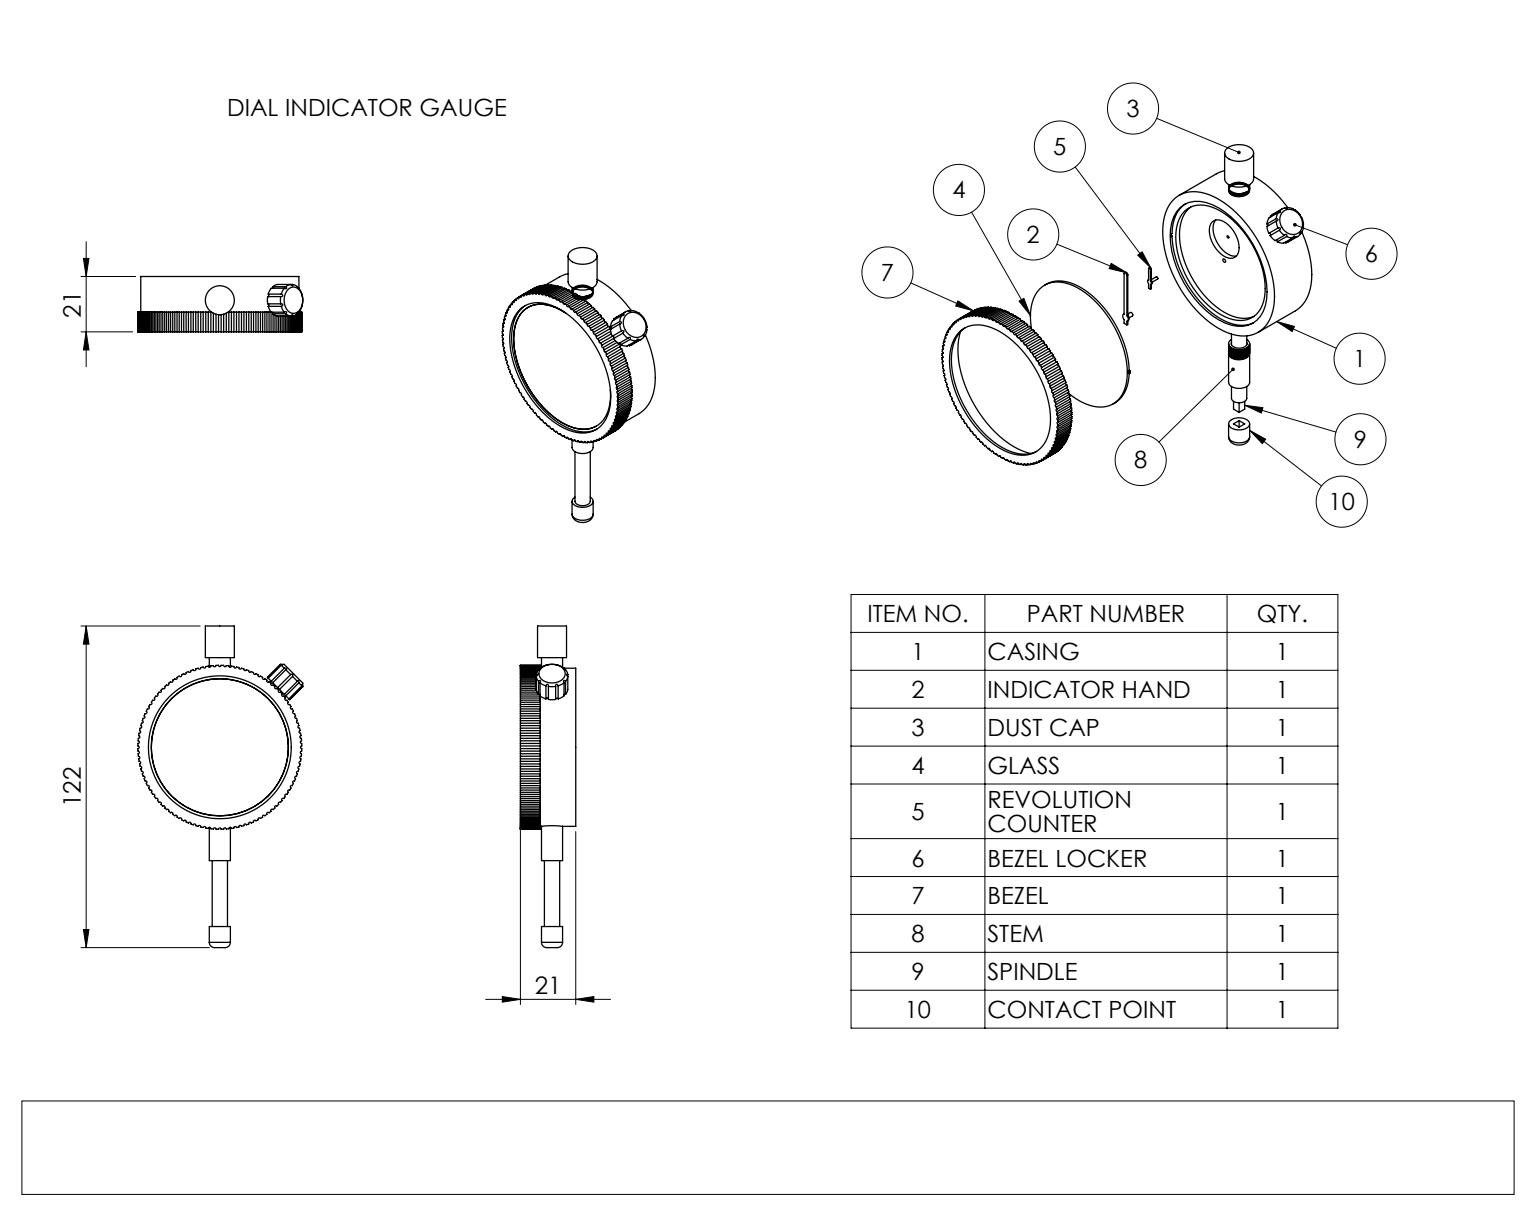
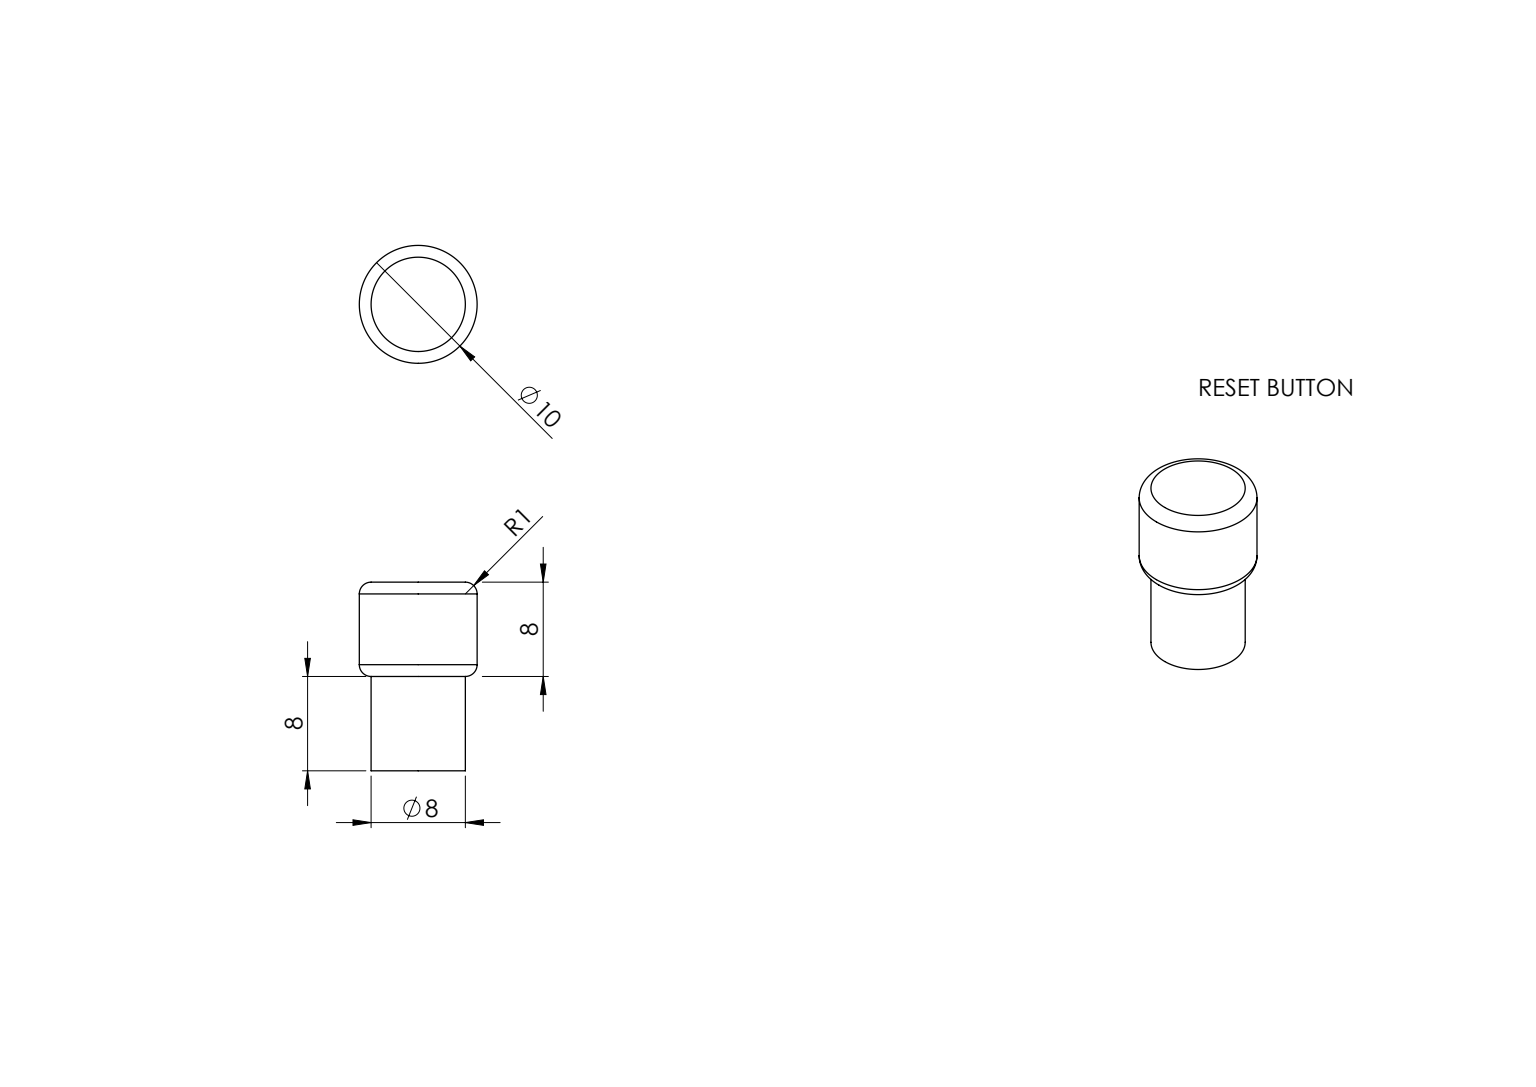
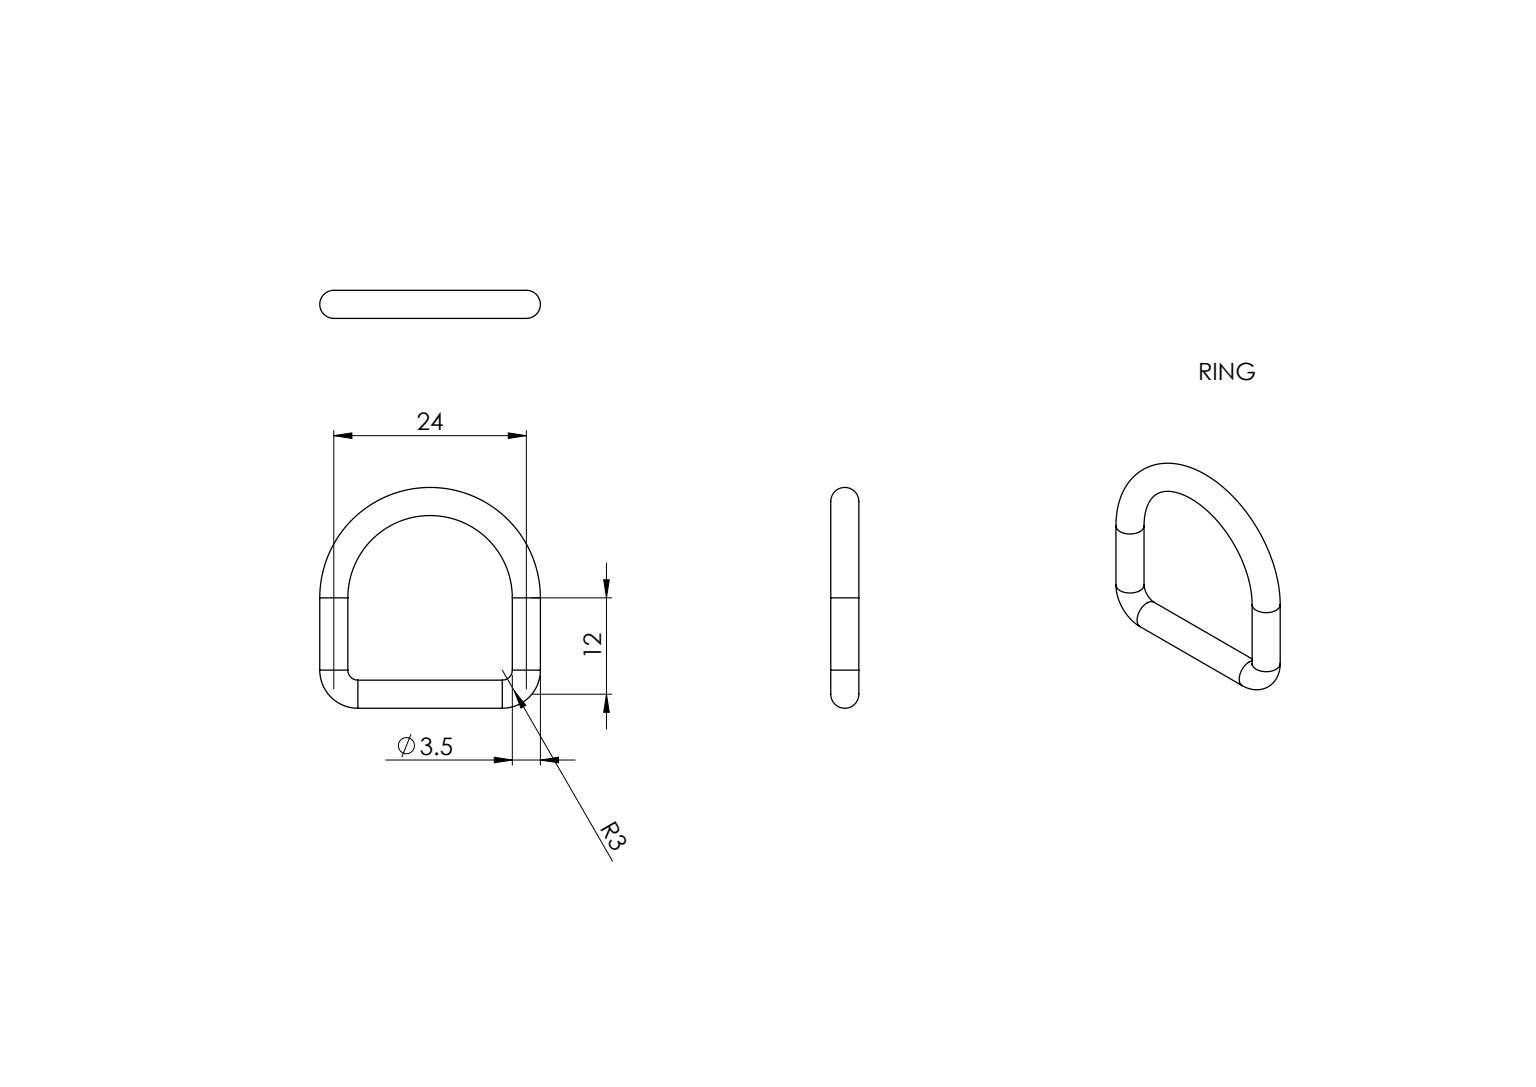
ISO-10303-21;
HEADER;
FILE_DESCRIPTION (('STEP AP214'),
    '1' );
FILE_NAME ('MAS-166',
    '2026-10-26T12:50:16',
    ( '' ),
    ( '' ),
    'SwSTEP 2.0',
    'SolidWorks 2026',
    '' );
FILE_SCHEMA (( 'AUTOMOTIVE_DESIGN' ));
ENDSEC;

DATA;
#1 = AXIS2_PLACEMENT_3D ( 'NONE', #24942, #2719, #13181 ) ;
#2 = CARTESIAN_POINT ( 'NONE',  ( -3.756430356249997882, -11.16877607737301226, 2.653124999385483296 ) ) ;
#3 = CARTESIAN_POINT ( 'NONE',  ( 2.000000000000003997, -5.535898384862238508, 4.518749998770967835 ) ) ;
#4 = SHAPE_REPRESENTATION_RELATIONSHIP ( 'NONE' , 'NONE' ,  #4483, #7868 ) ;
#5 = CARTESIAN_POINT ( 'NONE',  ( -3.756430356249995661, 28.14062499938548356, 6.831223922626973533 ) ) ;
#6 = AXIS2_PLACEMENT_3D ( 'NONE', #4398, #870, #8851 ) ;
#7 = CARTESIAN_POINT ( 'NONE',  ( -3.137519842735244810E-15, 26.85624999877096641, 4.999999999999991118 ) ) ;
#8 = CARTESIAN_POINT ( 'NONE',  ( 4.000000000000003553, -8.999999999999992895, 1.743749998770967924 ) ) ;
#9 = CARTESIAN_POINT ( 'NONE',  ( 2.620986760973688460E-15, -13.61880215351699874, 3.037499999999999201 ) ) ;
#10 = DIRECTION ( 'NONE',  ( 0.000000000000000000, 0.000000000000000000, -1.000000000000000000 ) ) ;
#11 = CARTESIAN_POINT ( 'NONE',  ( 4.000000000000003553, -8.999999999999992895, 2.643749998770966059 ) ) ;
#12 = DIRECTION ( 'NONE',  ( 1.000000000000000000, 0.000000000000000000, 0.000000000000000000 ) ) ;
#13 = CARTESIAN_POINT ( 'NONE',  ( 3.999999999999996003, -29.63124999877096499, 6.690598923241487306 ) ) ;
#14 = CARTESIAN_POINT ( 'NONE',  ( -1.878215178124995832, 27.65312499938548640, 5.746835883940462963 ) ) ;
#15 = CARTESIAN_POINT ( 'NONE',  ( 1.999999999999995781, -26.05000000000000071, 5.535898384862237620 ) ) ;
#16 = EDGE_CURVE ( 'NONE', #18357, #14663, #23368, .T. ) ;
#17 = CIRCLE ( 'NONE', #17974, 0.5000000000000003331 ) ;
#18 = CARTESIAN_POINT ( 'NONE',  ( 0.000000000000000000, 0.000000000000000000, 1.000000000000000000 ) ) ;
#19 = CARTESIAN_POINT ( 'NONE',  ( 3.469446951953614189E-15, 35.50000000000000711, 8.999999999999992895 ) ) ;
#20 = ORIENTED_EDGE ( 'NONE', *, *, #7327, .F. ) ;
#21 = CARTESIAN_POINT ( 'NONE',  ( -4.000000000000001776, -29.01249999999999929, 11.30940107675849760 ) ) ;
#23 = ORIENTED_EDGE ( 'NONE', *, *, #8423, .T. ) ;
#22 = CARTESIAN_POINT ( 'NONE',  ( 1.878215178124995832, -29.34062499938548285, 5.746835883940462963 ) ) ;
#24 = AXIS2_PLACEMENT_3D ( 'NONE', #8722, #14489, #16466 ) ;
#25 = ORIENTED_EDGE ( 'NONE', *, *, #21709, .F. ) ;
#26 = CARTESIAN_POINT ( 'NONE',  ( 3.959305671612554781E-15, 40.00000000000000000, 12.99999999999999289 ) ) ;
#27 = VERTEX_POINT ( 'NONE', #19559 ) ;
#28 = CARTESIAN_POINT ( 'NONE',  ( -1.878215178125000939, -26.86562499938548498, 12.25316411605952283 ) ) ;
#29 = ORIENTED_EDGE ( 'NONE', *, *, #15667, .T. ) ;
#30 = CYLINDRICAL_SURFACE ( 'NONE', #8395, 1.500000000000000222 ) ;
#31 = AXIS2_PLACEMENT_3D ( 'NONE', #2511, #8267, #24218 ) ;
#32 = VERTEX_POINT ( 'NONE', #17367 ) ;
#33 = CARTESIAN_POINT ( 'NONE',  ( 2.610164000359269210, 29.83019057377770622, 12.11182326528050623 ) ) ;
#34 = CARTESIAN_POINT ( 'NONE',  ( 3.756430356250003211, 25.74062499938548498, 6.831223922626973533 ) ) ;
#35 = CIRCLE ( 'NONE', #17990, 0.5000000000000006661 ) ;
#36 = CARTESIAN_POINT ( 'NONE',  ( 3.756430356250004099, -6.831223922626973533, 1.190624999385485383 ) ) ;
#37 = CARTESIAN_POINT ( 'NONE',  ( -1.859271017917182139E-15, -26.18124999877096570, 12.99999999999999289 ) ) ;
#38 = CARTESIAN_POINT ( 'NONE',  ( 20.96136040992792715, 18.30516303196848327, 12.25316411605952283 ) ) ;
#39 = CIRCLE ( 'NONE', #22153, 31.10000000000000142 ) ;
#40 = CARTESIAN_POINT ( 'NONE',  ( 7.901901826148023498E-15, 27.53124999877097068, 12.99999999999999112 ) ) ;
#41 = AXIS2_PLACEMENT_3D ( 'NONE', #20683, #20557, #10217 ) ;
#42 = SURFACE_SIDE_STYLE ('',( #19895 ) ) ;
#43 = APPLICATION_PROTOCOL_DEFINITION ( 'draft international standard', 'automotive_design', 1998, #21129 ) ;
#44 = EDGE_CURVE ( 'NONE', #18967, #21735, #3508, .T. ) ;
#45 = CARTESIAN_POINT ( 'NONE',  ( 2.620986760973688460E-15, 28.48750000000000071, 13.61880215351699874 ) ) ;
#46 = CONICAL_SURFACE ( 'NONE', #10212, 5.000000000000000888, 0.7853981633974445042 ) ;
#47 = CIRCLE ( 'NONE', #3373, 31.10000000000000142 ) ;
#48 = DIRECTION ( 'NONE',  ( -0.7071067811865463515, 0.7071067811865487940, 0.000000000000000000 ) ) ;
#49 = CARTESIAN_POINT ( 'NONE',  ( -10.98232076577242466, -29.09636799667071116, 1.000000000000000000 ) ) ;
#50 = CARTESIAN_POINT ( 'NONE',  ( -1.071796769724487675, -29.53615380933863221, 4.999999999999988454 ) ) ;
#51 = VERTEX_POINT ( 'NONE', #10384 ) ;
#52 = ORIENTED_EDGE ( 'NONE', *, *, #23161, .T. ) ;
#53 = CARTESIAN_POINT ( 'NONE',  ( -3.999999999999996447, 29.63124999877097210, 6.690598923241487306 ) ) ;
#54 = EDGE_CURVE ( 'NONE', #21865, #6150, #14230, .T. ) ;
#55 = CIRCLE ( 'NONE', #14670, 0.5000000000000005551 ) ;
#56 = VERTEX_POINT ( 'NONE', #24269 ) ;
#57 = CARTESIAN_POINT ( 'NONE',  ( 1.071796769724492338, 29.80134618820330417, 12.99999999999999467 ) ) ;
#58 = CARTESIAN_POINT ( 'NONE',  ( -3.756430356249996994, 25.47812499938548569, 8.999999999999992895 ) ) ;
#59 = DIRECTION ( 'NONE',  ( 0.000000000000000000, 1.000000000000000000, 0.000000000000000000 ) ) ;
#60 = CARTESIAN_POINT ( 'NONE',  ( -9.610428525061097460, -29.57785765677920509, -6.500000000000000000 ) ) ;
#61 = ADVANCED_FACE ( 'NONE', ( #4267 ), #12239, .F. ) ;
#62 = ORIENTED_EDGE ( 'NONE', *, *, #6026, .F. ) ;
#63 = VECTOR ( 'NONE', #7567, 1000.000000000000000 ) ;
#64 = ORIENTED_EDGE ( 'NONE', *, *, #14205, .F. ) ;
#65 = ADVANCED_FACE ( 'NONE', ( #4510 ), #16441, .F. ) ;
#66 = DIRECTION ( 'NONE',  ( 0.000000000000000000, 0.000000000000000000, 1.000000000000000000 ) ) ;
#67 =( BOUNDED_CURVE ( )  B_SPLINE_CURVE ( 2, ( #11399, #18754, #8825, #845, #17301 ),
 .UNSPECIFIED., .F., .F. ) 
 B_SPLINE_CURVE_WITH_KNOTS ( ( 3, 2, 3 ),
 ( 0.000000000000000000, 0.01666666666666666644, 0.02500000000000000486 ),
 .UNSPECIFIED. ) 
 CURVE ( )  GEOMETRIC_REPRESENTATION_ITEM ( )  RATIONAL_B_SPLINE_CURVE ( ( 1.000000000000000000, 0.8660254037844387076, 1.000000000000000000, 0.9330127018922194093, 0.9330127018922194093 ) ) 
 REPRESENTATION_ITEM ( '' )  );
#68 = CARTESIAN_POINT ( 'NONE',  ( -3.756430356249996994, 26.26562499938548711, 8.999999999999992895 ) ) ;
#69 = CARTESIAN_POINT ( 'NONE',  ( -3.756430356249997882, 29.45312499938549067, 11.16877607737301048 ) ) ;
#70 = AXIS2_PLACEMENT_3D ( 'NONE', #11835, #22027, #12224 ) ;
#71 = CARTESIAN_POINT ( 'NONE',  ( -2.000000000000003997, -26.87500000000000355, 5.535898384862238508 ) ) ;
#72 = DIRECTION ( 'NONE',  ( 1.000000000000000000, 0.000000000000000000, 0.000000000000000000 ) ) ;
#73 = CARTESIAN_POINT ( 'NONE',  ( 4.000000000000002665, 27.21250000000000568, 11.30940107675849760 ) ) ;
#74 =( BOUNDED_CURVE ( )  B_SPLINE_CURVE ( 2, ( #2295, #21785, #5959, #10252, #8301, #13672, #11709 ),
 .UNSPECIFIED., .F., .F. ) 
 B_SPLINE_CURVE_WITH_KNOTS ( ( 3, 2, 2, 3 ),
 ( 0.8999999999999996891, 0.9166666666666665186, 0.9333333333333335702, 0.9500000000000003997 ),
 .UNSPECIFIED. ) 
 CURVE ( )  GEOMETRIC_REPRESENTATION_ITEM ( )  RATIONAL_B_SPLINE_CURVE ( ( 1.000000000000002665, 0.8660254037844360431, 1.000000000000000000, 0.8660254037844387076, 1.000000000000000000, 0.8660254037844351549, 1.000000000000003553 ) ) 
 REPRESENTATION_ITEM ( '' )  );
#75 = TOROIDAL_SURFACE ( 'NONE', #19699, 2.000000000000000000, 2.000000000000000000 ) ;
#76 = CARTESIAN_POINT ( 'NONE',  ( -3.756430356249996994, 26.26562499938548711, 8.999999999999992895 ) ) ;
#77 =( LENGTH_UNIT ( ) NAMED_UNIT ( * ) SI_UNIT ( .MILLI., .METRE. ) );
#78 = VECTOR ( 'NONE', #8219, 1000.000000000000000 ) ;
#79 = AXIS2_PLACEMENT_3D ( 'NONE', #15726, #13515, #3680 ) ;
#80 = CARTESIAN_POINT ( 'NONE',  ( -3.469446951953614189E-15, -30.00000000000000355, 4.999999999999992006 ) ) ;
#81 = DIRECTION ( 'NONE',  ( 0.000000000000000000, 0.000000000000000000, 1.000000000000000000 ) ) ;
#82 = CARTESIAN_POINT ( 'NONE',  ( 15.67125403804690009, 21.32810828753921228, 11.30940107675849404 ) ) ;
#83 = CARTESIAN_POINT ( 'NONE',  ( -23.01025686871652809, -20.92219106202034595, 1.000000000000000000 ) ) ;
#84 = DIRECTION ( 'NONE',  ( 0.000000000000000000, 1.000000000000000000, 0.000000000000000000 ) ) ;
#85 = CARTESIAN_POINT ( 'NONE',  ( 0.000000000000000000, 10.00000000000000000, 13.00000000000000178 ) ) ;
#86 = CIRCLE ( 'NONE', #1339, 31.10000000000000142 ) ;
#87 = CARTESIAN_POINT ( 'NONE',  ( 3.756430356250004987, 25.19687499938549280, 8.999999999999992895 ) ) ;
#88 = CARTESIAN_POINT ( 'NONE',  ( 17.82559248041273037, 23.13798723633140142, 8.999999999999992895 ) ) ;
#89 = VERTEX_POINT ( 'NONE', #21923 ) ;
#90 = CARTESIAN_POINT ( 'NONE',  ( 4.000000000000003553, 27.19374999877096855, 8.999999999999992895 ) ) ;
#91 = CARTESIAN_POINT ( 'NONE',  ( -3.752267015613588906E-15, -27.36250000000000071, 4.381197846482986158 ) ) ;
#93 = ORIENTED_EDGE ( 'NONE', *, *, #14257, .T. ) ;
#92 = CARTESIAN_POINT ( 'NONE',  ( 4.006172263299091013E-15, 27.16562499938547859, 4.662447845253954171 ) ) ;
#94 = CARTESIAN_POINT ( 'NONE',  ( 3.756430356250002323, 29.26562499938548356, 11.16877607737301403 ) ) ;
#95 = AXIS2_PLACEMENT_3D ( 'NONE', #9918, #10180, #22078 ) ;
#96 = DIRECTION ( 'NONE',  ( 0.000000000000000000, 1.000000000000000000, 0.000000000000000000 ) ) ;
#97 = CYLINDRICAL_SURFACE ( 'NONE', #3366, 0.5000000000000004441 ) ;
#98 = ORIENTED_EDGE ( 'NONE', *, *, #19921, .T. ) ;
#99 = ORIENTED_EDGE ( 'NONE', *, *, #21927, .F. ) ;
#100 = ADVANCED_FACE ( 'NONE', ( #14466 ), #6356, .T. ) ;
#101 = CARTESIAN_POINT ( 'NONE',  ( 3.756430356250002323, 27.35312499938548569, 11.16877607737301226 ) ) ;
#102 = ADVANCED_FACE ( 'NONE', ( #22181 ), #12564, .T. ) ;
#103 = CARTESIAN_POINT ( 'NONE',  ( 2.672651547586948120E-15, -13.33755215474603162, 2.278124999385481964 ) ) ;
#104 = AXIS2_PLACEMENT_3D ( 'NONE', #18680, #4701, #2727 ) ;
#105 = EDGE_CURVE ( 'NONE', #8835, #13216, #4631, .T. ) ;
#106 = CIRCLE ( 'NONE', #18070, 0.4999999999999998890 ) ;
#107 = EDGE_CURVE ( 'NONE', #585, #4269, #18005, .T. ) ;
#108 = FACE_OUTER_BOUND ( 'NONE', #8911, .T. ) ;
#109 = SHAPE_REPRESENTATION_RELATIONSHIP ( 'NONE' , 'NONE' ,  #19829, #5978 ) ;
#110 = CARTESIAN_POINT ( 'NONE',  ( 1.500000000000001776, -10.49999999999999289, 4.999999999999993783 ) ) ;
#111 = FACE_OUTER_BOUND ( 'NONE', #10588, .T. ) ;
#112 = AXIS2_PLACEMENT_3D ( 'NONE', #10691, #2608, #22745 ) ;
#113 = EDGE_CURVE ( 'NONE', #22373, #14800, #20983, .T. ) ;
#114 = DIRECTION ( 'NONE',  ( -0.000000000000000000, -1.000000000000000000, -0.000000000000000000 ) ) ;
#115 = CARTESIAN_POINT ( 'NONE',  ( 3.718542035834364277E-15, 25.11250000000000782, 4.999999999999992006 ) ) ;
#116 = CARTESIAN_POINT ( 'NONE',  ( 23.35662086519912606, 17.69976661570667176, 6.690598923241489970 ) ) ;
#117 = ORIENTED_EDGE ( 'NONE', *, *, #18852, .F. ) ;
#118 = CARTESIAN_POINT ( 'NONE',  ( -5.395002858709908367, 38.91217497027906802, 10.45656796931105426 ) ) ;
#119 = CARTESIAN_POINT ( 'NONE',  ( 3.472074595960224386, 29.79875828571876184, 6.996763648122163559 ) ) ;
#120 = CARTESIAN_POINT ( 'NONE',  ( 3.756430356250002323, 27.01562499938548356, 11.16877607737301226 ) ) ;
#121 = AXIS2_PLACEMENT_3D ( 'NONE', #5758, #23946, #12025 ) ;
#122 = CARTESIAN_POINT ( 'NONE',  ( -3.178742173564956808, 29.83148068024111410, 6.557713274934318548 ) ) ;
#123 = CARTESIAN_POINT ( 'NONE',  ( 3.469446951953614189E-15, 35.50000000000000711, 4.999999999999992006 ) ) ;
#124 = CARTESIAN_POINT ( 'NONE',  ( 3.370160183775990248, 38.97860908142764913, 13.37397733810513856 ) ) ;
#125 = VERTEX_POINT ( 'NONE', #4004 ) ;
#126 = CARTESIAN_POINT ( 'NONE',  ( 2.000000000000005329, 26.81874999877097210, 5.535898384862238508 ) ) ;
#127 = CARTESIAN_POINT ( 'NONE',  ( 3.469446951953614189E-15, 35.50000000000000711, 4.999999999999992006 ) ) ;
#128 = LINE ( 'NONE', #11881, #5846 ) ;
#130 = VERTEX_POINT ( 'NONE', #22041 ) ;
#129 = DIRECTION ( 'NONE',  ( 1.000000000000000000, 0.000000000000000000, 0.000000000000000000 ) ) ;
#131 = ORIENTED_EDGE ( 'NONE', *, *, #19522, .T. ) ;
#132 = VERTEX_POINT ( 'NONE', #22432 ) ;
#133 = ORIENTED_EDGE ( 'NONE', *, *, #9364, .F. ) ;
#134 = DIRECTION ( 'NONE',  ( 0.2486898871648519360, -0.9685831611286318532, 0.000000000000000000 ) ) ;
#135 = LINE ( 'NONE', #23787, #14039 ) ;
#136 = EDGE_CURVE ( 'NONE', #11885, #9403, #6717, .T. ) ;
#137 = AXIS2_PLACEMENT_3D ( 'NONE', #2400, #6189, #455 ) ;
#138 = CARTESIAN_POINT ( 'NONE',  ( 22.67092431280594056, 21.28941499438218088, 1.000000000000000000 ) ) ;
#139 = CARTESIAN_POINT ( 'NONE',  ( -1.878215178124998275, 25.89062499938549067, 12.25316411605951927 ) ) ;
#140 = VECTOR ( 'NONE', #15561, 1000.000000000000000 ) ;
#141 = CARTESIAN_POINT ( 'NONE',  ( -3.756430356249997882, -11.16877607737301226, 4.453124999385482674 ) ) ;
#142 = CARTESIAN_POINT ( 'NONE',  ( 1.878215178125004048, -5.746835883940462963, 0.3281249993854831737 ) ) ;
#143 = CARTESIAN_POINT ( 'NONE',  ( -3.756430356249995661, 26.22812499938548214, 6.831223922626973533 ) ) ;
#144 = EDGE_CURVE ( 'NONE', #7410, #22395, #341, .T. ) ;
#145 = DIRECTION ( 'NONE',  ( 0.000000000000000000, 0.000000000000000000, -1.000000000000000000 ) ) ;
#146 = LINE ( 'NONE', #8118, #8436 ) ;
#147 = CIRCLE ( 'NONE', #18512, 0.4999999999999997224 ) ;
#148 = CARTESIAN_POINT ( 'NONE',  ( -3.756430356249997438, 26.30312499938548854, 11.16877607737301048 ) ) ;
#149 = DIRECTION ( 'NONE',  ( -0.7071067811865487940, -0.7071067811865463515, 0.000000000000000000 ) ) ;
#150 = CARTESIAN_POINT ( 'NONE',  ( -3.369928719974892281E-15, -25.50624999877096855, 4.999999999999992006 ) ) ;
#151 = DIRECTION ( 'NONE',  ( -0.000000000000000000, 0.000000000000000000, 1.000000000000000000 ) ) ;
#152 = CARTESIAN_POINT ( 'NONE',  ( -4.000000000000003553, -28.99374999877096926, 8.999999999999992895 ) ) ;
#153 = CARTESIAN_POINT ( 'NONE',  ( -3.756430356249996994, 28.62812499938548427, 8.999999999999992895 ) ) ;
#154 = AXIS2_PLACEMENT_3D ( 'NONE', #12888, #20866, #10658 ) ;
#155 = CARTESIAN_POINT ( 'NONE',  ( 1.071796769724497222, 28.00134618820329990, 12.99999999999998757 ) ) ;
#156 = CARTESIAN_POINT ( 'NONE',  ( -3.834746474454188013E-15, -25.95624999877096428, 4.999999999999992006 ) ) ;
#157 = ORIENTED_EDGE ( 'NONE', *, *, #19996, .F. ) ;
#158 = DIRECTION ( 'NONE',  ( 0.4817536741017267032, 0.8763066800438573667, 0.000000000000000000 ) ) ;
#160 = ORIENTED_EDGE ( 'NONE', *, *, #14930, .T. ) ;
#159 = CARTESIAN_POINT ( 'NONE',  ( -2.672651547586948120E-15, -29.52812499938548285, 13.33755215474603162 ) ) ;
#161 = VERTEX_POINT ( 'NONE', #10530 ) ;
#162 = EDGE_LOOP ( 'NONE', ( #20423, #8282, #5140, #7710 ) ) ;
#163 = ORIENTED_EDGE ( 'NONE', *, *, #23989, .T. ) ;
#164 = ORIENTED_EDGE ( 'NONE', *, *, #21623, .F. ) ;
#165 = DIRECTION ( 'NONE',  ( -1.000000000000000000, 0.000000000000000000, 0.000000000000000000 ) ) ;
#166 = ORIENTED_EDGE ( 'NONE', *, *, #16755, .F. ) ;
#167 = CARTESIAN_POINT ( 'NONE',  ( 1.859271017917182139E-15, 29.78124999877096712, 12.99999999999999289 ) ) ;
#168 = CARTESIAN_POINT ( 'NONE',  ( 3.756430356250003211, 26.19062499938548783, 6.831223922626973533 ) ) ;
#169 = CIRCLE ( 'NONE', #23535, 31.10000000000000142 ) ;
#170 = EDGE_CURVE ( 'NONE', #5115, #14942, #12104, .T. ) ;
#171 = CARTESIAN_POINT ( 'NONE',  ( 1.878215178125000939, -12.25316411605952283, 3.778124999385484628 ) ) ;
#172 = FACE_OUTER_BOUND ( 'NONE', #2936, .T. ) ;
#173 = CARTESIAN_POINT ( 'NONE',  ( 18.33395301051795911, 18.33395301051789161, 13.33755215474602984 ) ) ;
#174 = CARTESIAN_POINT ( 'NONE',  ( 17.58044234725058175, 23.23729659674288683, 11.30940107675849404 ) ) ;
#175 = LINE ( 'NONE', #12048, #20896 ) ;
#176 = CARTESIAN_POINT ( 'NONE',  ( 3.756430356250003655, -8.999999999999992895, 0.5906249993854819635 ) ) ;
#177 = CARTESIAN_POINT ( 'NONE',  ( 4.000000000000003553, 28.18750000000000000, 6.690598923241489970 ) ) ;
#178 = CARTESIAN_POINT ( 'NONE',  ( 3.756430356250003211, 28.77812499938548285, 6.831223922626973533 ) ) ;
#179 = DIRECTION ( 'NONE',  ( -0.000000000000000000, 0.000000000000000000, -1.000000000000000000 ) ) ;
#180 = DIRECTION ( 'NONE',  ( 1.000000000000000000, 0.000000000000000000, 0.000000000000000000 ) ) ;
#181 =( BOUNDED_CURVE ( )  B_SPLINE_CURVE ( 2, ( #6217, #22433, #20464, #14467, #6482, #24270, #342, #4511, #8455 ),
 .UNSPECIFIED., .F., .T. ) 
 B_SPLINE_CURVE_WITH_KNOTS ( ( 3, 2, 2, 2, 3 ),
 ( 0.02500000000000000139, 0.03333333333333333287, 0.05000000000000000278, 0.06666666666666666574, 0.07500000000000001110 ),
 .UNSPECIFIED. ) 
 CURVE ( )  GEOMETRIC_REPRESENTATION_ITEM ( )  RATIONAL_B_SPLINE_CURVE ( ( 0.9330127018922194093, 0.9330127018922194093, 1.000000000000000000, 0.8660254037844387076, 1.000000000000000000, 0.8660254037844387076, 1.000000000000000000, 0.9330127018922191873, 0.9330127018922192983 ) ) 
 REPRESENTATION_ITEM ( '' )  );
#182 = AXIS2_PLACEMENT_3D ( 'NONE', #20476, #4664, #8852 ) ;
#183 = ORIENTED_EDGE ( 'NONE', *, *, #8865, .T. ) ;
#184 = VERTEX_POINT ( 'NONE', #16301 ) ;
#185 = CARTESIAN_POINT ( 'NONE',  ( -1.878215178124994722, 25.40312499938548996, 5.746835883940462963 ) ) ;
#186 = ORIENTED_EDGE ( 'NONE', *, *, #6669, .T. ) ;
#187 = DIRECTION ( 'NONE',  ( -0.000000000000000000, -0.000000000000000000, 1.000000000000000000 ) ) ;
#188 = CARTESIAN_POINT ( 'NONE',  ( 4.000000000000003553, 29.44374999877096855, 8.999999999999992895 ) ) ;
#189 = CARTESIAN_POINT ( 'NONE',  ( -3.999999999999996447, 29.23750000000001137, 6.690598923241487306 ) ) ;
#190 = DIRECTION ( 'NONE',  ( -0.2486898871648584586, -0.9685831611286301879, 0.000000000000000000 ) ) ;
#191 = ORIENTED_EDGE ( 'NONE', *, *, #21291, .T. ) ;
#192 = DIRECTION ( 'NONE',  ( 1.000000000000000000, -0.000000000000000000, -0.000000000000000000 ) ) ;
#193 = ORIENTED_EDGE ( 'NONE', *, *, #13144, .T. ) ;
#194 = LINE ( 'NONE', #20580, #24770 ) ;
#195 = CARTESIAN_POINT ( 'NONE',  ( -3.756430356249997882, 27.20312499938548001, 11.16877607737301226 ) ) ;
#196 = FACE_OUTER_BOUND ( 'NONE', #24755, .T. ) ;
#197 = EDGE_CURVE ( 'NONE', #20602, #23121, #20077, .T. ) ;
#198 = PRODUCT_DEFINITION_FORMATION_WITH_SPECIFIED_SOURCE ( 'ANY', '', #10050, .NOT_KNOWN. ) ;
#199 = DIRECTION ( 'NONE',  ( 0.000000000000000000, 0.000000000000000000, 1.000000000000000000 ) ) ;
#200 = CARTESIAN_POINT ( 'NONE',  ( -1.859271017917182139E-15, 26.46249999999999858, 4.999999999999991118 ) ) ;
#201 = CARTESIAN_POINT ( 'NONE',  ( 15.35955758102464408, 20.67195233694332401, 8.999999999999992895 ) ) ;
#202 = EDGE_CURVE ( 'NONE', #18727, #446, #20080, .T. ) ;
#203 = CARTESIAN_POINT ( 'NONE',  ( -1.878215178124998497, 25.44062499938548427, 12.25316411605951927 ) ) ;
#204 = EDGE_CURVE ( 'NONE', #4422, #2251, #3256, .T. ) ;
#205 = CARTESIAN_POINT ( 'NONE',  ( 3.999999999999996447, -28.76874999877096784, 8.999999999999992895 ) ) ;
#206 = CARTESIAN_POINT ( 'NONE',  ( 20.78010053211970032, 20.78010053211962926, 13.61880215351699874 ) ) ;
#207 = CARTESIAN_POINT ( 'NONE',  ( -30.85476721088022600, 3.897863563850190616, 1.000000000000000000 ) ) ;
#208 = EDGE_CURVE ( 'NONE', #13339, #3186, #993, .T. ) ;
#209 = DIRECTION ( 'NONE',  ( 0.000000000000000000, -0.000000000000000000, -1.000000000000000000 ) ) ;
#210 = CARTESIAN_POINT ( 'NONE',  ( 21.65072575558658130, 18.82229863084031507, 5.535898384862238508 ) ) ;
#211 = DIRECTION ( 'NONE',  ( 0.000000000000000000, -0.000000000000000000, 1.000000000000000000 ) ) ;
#212 = FACE_BOUND ( 'NONE', #16233, .T. ) ;
#213 = ORIENTED_EDGE ( 'NONE', *, *, #20465, .F. ) ;
#214 = CARTESIAN_POINT ( 'NONE',  ( -1.999999999999995781, 28.69374999877096855, 5.535898384862237620 ) ) ;
#215 = CARTESIAN_POINT ( 'NONE',  ( -4.000000000000003553, -28.18750000000000000, 6.690598923241489970 ) ) ;
#217 = ORIENTED_EDGE ( 'NONE', *, *, #6066, .T. ) ;
#216 = CARTESIAN_POINT ( 'NONE',  ( -1.878215178124999829, 26.90312499938548640, 12.25316411605951927 ) ) ;
#218 = CARTESIAN_POINT ( 'NONE',  ( 3.756430356250002323, 27.46562499938548640, 11.16877607737301403 ) ) ;
#219 = CARTESIAN_POINT ( 'NONE',  ( 23.82728881686095335, 18.17043456736849549, 8.999999999999992895 ) ) ;
#220 = CARTESIAN_POINT ( 'NONE',  ( -3.999999999999997335, 27.90624999877097068, 11.30940107675849404 ) ) ;
#221 = ORIENTED_EDGE ( 'NONE', *, *, #3705, .F. ) ;
#222 = ORIENTED_EDGE ( 'NONE', *, *, #22140, .F. ) ;
#223 =( NAMED_UNIT ( * ) PLANE_ANGLE_UNIT ( ) SI_UNIT ( $, .RADIAN. ) );
#224 = CARTESIAN_POINT ( 'NONE',  ( -3.756430356249998326, 28.10312499938548569, 11.16877607737301226 ) ) ;
#225 =( BOUNDED_SURFACE ( )  B_SPLINE_SURFACE ( 1, 2, ( 
 ( #23282, #15066, #19226, #12835, #25256, #13355, #9305, #1328, #23041, #11121, #11003, #7335, #805, #4859, #6951, #3034, #14929, #17290, #15314, #5365, #6826, #4989, #3408, #23165, #3271, #1184, #20809, #11245, #18713, #14809, #25127, #22903, #22782, #7213, #5128, #3154, #5245, #18859, #15195, #2891, #949, #8926, #12968, #18983, #9042, #17024, #13105, #21078, #19100, #11896, #19864, #23669, #17408, #3538, #9928, #7455, #23415, #17792, #7595, #5502, #13493, #15443, #3926, #23933, #5746, #11511, #11387, #7721, #9545, #15581, #17532, #25759, #1963, #17913, #11771, #13997, #19750, #5, #5885, #21462, #15967, #25506, #15705, #23549, #1848, #23795, #25372, #17671, #13730, #5631, #19480, #7979, #6016, #21968, #13611, #19361, #1456, #1574, #21577, #3656, #11632, #19609, #21708, #3793, #1713, #9427, #9810, #9687, #25639, #7840, #15824, #13869, #21843, #20128, #2470, #14641, #12011, #18436, #18572, #4433, #18301 ),
 ( #24054, #14507, #12542, #2614, #10441, #2229, #2094, #531, #16352, #14392, #16485, #4175, #8503, #22479, #10573, #24447, #10187, #4559, #4044, #6524, #20373, #20519, #19988, #654, #8623, #24321, #10061, #22086, #16600, #143, #16090, #24562, #267, #6138, #14122, #8116, #6652, #18060, #6401, #12154, #18184, #393, #8235, #16212, #24181, #6269, #14261, #22228, #12407, #4313, #12287, #20253, #2351, #10306, #8362, #22349, #1037, #20778, #13070, #9481, #10697, #2998, #18952, #8890, #4827, #13549, #5568, #15512, #911, #19534, #11566, #772, #10827, #8745, #16735, #4951, #7655, #10966, #14776, #22871, #18820, #12933, #17460, #9011, #22621, #22752, #12804, #21513, #16992, #2857, #24957, #14897, #16874, #24838, #7039, #24705, #25571, #25432, #6915, #12683, #18684, #9614, #1636, #15027, #23481, #21048, #20911, #20652, #3123, #23005, #5092, #7517, #11091, #19070, #3595, #17594, #1512, #4708, #2735, #6791, #18129 ) ),
 .UNSPECIFIED., .F., .F., .F. ) 
 B_SPLINE_SURFACE_WITH_KNOTS ( ( 2, 2 ),
 ( 3, 2, 2, 2, 2, 2, 2, 2, 2, 2, 2, 2, 2, 2, 2, 2, 2, 2, 2, 2, 2, 2, 2, 2, 2, 2, 2, 2, 2, 2, 2, 2, 2, 2, 2, 2, 2, 2, 2, 2, 2, 2, 2, 2, 2, 2, 2, 2, 2, 2, 2, 2, 2, 2, 2, 2, 2, 2, 2, 2, 3 ),
 ( 0.000000000000000000, 1.000000000000000000 ),
 ( 0.000000000000000000, 0.01666666666666666644, 0.03333333333333333287, 0.05000000000000000278, 0.06666666666666666574, 0.08333333333333332871, 0.1000000000000000056, 0.1166666666666666685, 0.1333333333333333315, 0.1499999999999999944, 0.1666666666666666574, 0.1833333333333333204, 0.2000000000000000111, 0.2166666666666666741, 0.2333333333333333370, 0.2500000000000000000, 0.2666666666666666630, 0.2833333333333333259, 0.2999999999999999889, 0.3166666666666666519, 0.3333333333333333148, 0.3499999999999999778, 0.3666666666666666408, 0.3833333333333333592, 0.4000000000000000222, 0.4166666666666666852, 0.4333333333333333481, 0.4500000000000000111, 0.4666666666666666741, 0.4833333333333333370, 0.5000000000000000000, 0.5166666666666667185, 0.5333333333333333259, 0.5500000000000000444, 0.5666666666666666519, 0.5833333333333333703, 0.5999999999999999778, 0.6166666666666666963, 0.6333333333333333037, 0.6500000000000000222, 0.6666666666666666297, 0.6833333333333333481, 0.6999999999999999556, 0.7166666666666666741, 0.7333333333333332815, 0.7500000000000000000, 0.7666666666666667185, 0.7833333333333333259, 0.8000000000000000444, 0.8166666666666666519, 0.8333333333333333703, 0.8499999999999999778, 0.8666666666666666963, 0.8833333333333333037, 0.9000000000000000222, 0.9166666666666666297, 0.9333333333333333481, 0.9499999999999999556, 0.9666666666666666741, 0.9833333333333332815, 1.000000000000000000 ),
 .UNSPECIFIED. ) 
 GEOMETRIC_REPRESENTATION_ITEM ( )  RATIONAL_B_SPLINE_SURFACE ( (
 ( 1.000000000000000000, 0.8660254037844387076, 1.000000000000000000, 0.8660254037844387076, 1.000000000000000000, 0.8660254037844387076, 1.000000000000000000, 0.8660254037844387076, 1.000000000000000000, 0.8660254037844387076, 1.000000000000000000, 0.8660254037844387076, 1.000000000000000000, 0.8660254037844387076, 1.000000000000000000, 0.8660254037844387076, 1.000000000000000000, 0.8660254037844387076, 1.000000000000000000, 0.8660254037844387076, 1.000000000000000000, 0.8660254037844387076, 1.000000000000000000, 0.8660254037844387076, 1.000000000000000000, 0.8660254037844387076, 1.000000000000000000, 0.8660254037844387076, 1.000000000000000000, 0.8660254037844387076, 1.000000000000000000, 0.8660254037844387076, 1.000000000000000000, 0.8660254037844387076, 1.000000000000000000, 0.8660254037844387076, 1.000000000000000000, 0.8660254037844387076, 1.000000000000000000, 0.8660254037844387076, 1.000000000000000000, 0.8660254037844387076, 1.000000000000000000, 0.8660254037844387076, 1.000000000000000000, 0.8660254037844387076, 1.000000000000000000, 0.8660254037844387076, 1.000000000000000000, 0.8660254037844387076, 1.000000000000000000, 0.8660254037844387076, 1.000000000000000000, 0.8660254037844387076, 1.000000000000000000, 0.8660254037844387076, 1.000000000000000000, 0.8660254037844387076, 1.000000000000000000, 0.8660254037844387076, 1.000000000000000000, 0.8660254037844387076, 1.000000000000000000, 0.8660254037844387076, 1.000000000000000000, 0.8660254037844387076, 1.000000000000000000, 0.8660254037844387076, 1.000000000000000000, 0.8660254037844387076, 1.000000000000000000, 0.8660254037844387076, 1.000000000000000000, 0.8660254037844387076, 1.000000000000000000, 0.8660254037844387076, 1.000000000000000000, 0.8660254037844387076, 1.000000000000000000, 0.8660254037844387076, 1.000000000000000000, 0.8660254037844387076, 1.000000000000000000, 0.8660254037844387076, 1.000000000000000000, 0.8660254037844387076, 1.000000000000000000, 0.8660254037844387076, 1.000000000000000000, 0.8660254037844387076, 1.000000000000000000, 0.8660254037844387076, 1.000000000000000000, 0.8660254037844387076, 1.000000000000000000, 0.8660254037844387076, 1.000000000000000000, 0.8660254037844387076, 1.000000000000000000, 0.8660254037844387076, 1.000000000000000000, 0.8660254037844387076, 1.000000000000000000, 0.8660254037844387076, 1.000000000000000000, 0.8660254037844387076, 1.000000000000000000, 0.8660254037844387076, 1.000000000000000000, 0.8660254037844387076, 1.000000000000000000, 0.8660254037844387076, 1.000000000000000000, 0.8660254037844387076, 1.000000000000000000, 0.8660254037844387076, 1.000000000000000000, 0.8660254037844387076, 1.000000000000000000, 0.8660254037844387076, 1.000000000000000000),
 ( 1.000000000000000000, 0.8660254037844387076, 1.000000000000000000, 0.8660254037844387076, 1.000000000000000000, 0.8660254037844387076, 1.000000000000000000, 0.8660254037844387076, 1.000000000000000000, 0.8660254037844387076, 1.000000000000000000, 0.8660254037844387076, 1.000000000000000000, 0.8660254037844387076, 1.000000000000000000, 0.8660254037844387076, 1.000000000000000000, 0.8660254037844387076, 1.000000000000000000, 0.8660254037844387076, 1.000000000000000000, 0.8660254037844387076, 1.000000000000000000, 0.8660254037844387076, 1.000000000000000000, 0.8660254037844387076, 1.000000000000000000, 0.8660254037844387076, 1.000000000000000000, 0.8660254037844387076, 1.000000000000000000, 0.8660254037844387076, 1.000000000000000000, 0.8660254037844387076, 1.000000000000000000, 0.8660254037844387076, 1.000000000000000000, 0.8660254037844387076, 1.000000000000000000, 0.8660254037844387076, 1.000000000000000000, 0.8660254037844387076, 1.000000000000000000, 0.8660254037844387076, 1.000000000000000000, 0.8660254037844387076, 1.000000000000000000, 0.8660254037844387076, 1.000000000000000000, 0.8660254037844387076, 1.000000000000000000, 0.8660254037844387076, 1.000000000000000000, 0.8660254037844387076, 1.000000000000000000, 0.8660254037844387076, 1.000000000000000000, 0.8660254037844387076, 1.000000000000000000, 0.8660254037844387076, 1.000000000000000000, 0.8660254037844387076, 1.000000000000000000, 0.8660254037844387076, 1.000000000000000000, 0.8660254037844387076, 1.000000000000000000, 0.8660254037844387076, 1.000000000000000000, 0.8660254037844387076, 1.000000000000000000, 0.8660254037844387076, 1.000000000000000000, 0.8660254037844387076, 1.000000000000000000, 0.8660254037844387076, 1.000000000000000000, 0.8660254037844387076, 1.000000000000000000, 0.8660254037844387076, 1.000000000000000000, 0.8660254037844387076, 1.000000000000000000, 0.8660254037844387076, 1.000000000000000000, 0.8660254037844387076, 1.000000000000000000, 0.8660254037844387076, 1.000000000000000000, 0.8660254037844387076, 1.000000000000000000, 0.8660254037844387076, 1.000000000000000000, 0.8660254037844387076, 1.000000000000000000, 0.8660254037844387076, 1.000000000000000000, 0.8660254037844387076, 1.000000000000000000, 0.8660254037844387076, 1.000000000000000000, 0.8660254037844387076, 1.000000000000000000, 0.8660254037844387076, 1.000000000000000000, 0.8660254037844387076, 1.000000000000000000, 0.8660254037844387076, 1.000000000000000000, 0.8660254037844387076, 1.000000000000000000, 0.8660254037844387076, 1.000000000000000000, 0.8660254037844387076, 1.000000000000000000, 0.8660254037844387076, 1.000000000000000000, 0.8660254037844387076, 1.000000000000000000, 0.8660254037844387076, 1.000000000000000000) ) ) 
 REPRESENTATION_ITEM ( '' )  SURFACE ( )  );
#226 = DIRECTION ( 'NONE',  ( 0.000000000000000000, 0.000000000000000000, 1.000000000000000000 ) ) ;
#227 = CARTESIAN_POINT ( 'NONE',  ( -3.756430356249996994, -8.999999999999992895, 3.515624999385482674 ) ) ;
#228 = CARTESIAN_POINT ( 'NONE',  ( -3.999999999999999112, 28.35624999877097707, 11.30940107675849404 ) ) ;
#229 = PRODUCT_DEFINITION ( 'UNKNOWN', '', #18569, #2861 ) ;
#230 = CIRCLE ( 'NONE', #3567, 26.00000000000000355 ) ;
#231 =( LENGTH_UNIT ( ) NAMED_UNIT ( * ) SI_UNIT ( .MILLI., .METRE. ) );
#232 = CARTESIAN_POINT ( 'NONE',  ( -30.12293631110050995, -7.734255490826679846, 1.000000000000000000 ) ) ;
#233 = DIRECTION ( 'NONE',  ( 1.000000000000000000, 0.000000000000000000, 0.000000000000000000 ) ) ;
#234 = CARTESIAN_POINT ( 'NONE',  ( 22.12360341637413441, 16.46674916688168366, 6.690598923241489970 ) ) ;
#235 = CARTESIAN_POINT ( 'NONE',  ( 21.07620149587250680, 15.41934724638005605, 11.30940107675849760 ) ) ;
#236 = CARTESIAN_POINT ( 'NONE',  ( -3.999999999999996447, 26.51874999877097494, 8.999999999999992895 ) ) ;
#237 = CARTESIAN_POINT ( 'NONE',  ( 16.26111872703749128, 21.57351348295617299, 11.16877607737301226 ) ) ;
#238 = CARTESIAN_POINT ( 'NONE',  ( 20.69613160098474580, 17.86770447623847957, 5.535898384862238508 ) ) ;
#239 = EDGE_CURVE ( 'NONE', #21040, #20500, #15911, .T. ) ;
#240 = ORIENTED_EDGE ( 'NONE', *, *, #11799, .T. ) ;
#241 = DIRECTION ( 'NONE',  ( -0.000000000000000000, -1.000000000000000000, -0.000000000000000000 ) ) ;
#242 = FACE_OUTER_BOUND ( 'NONE', #14530, .T. ) ;
#243 = CARTESIAN_POINT ( 'NONE',  ( 3.756430356250003655, 29.75312499938548783, 8.999999999999992895 ) ) ;
#244 = ADVANCED_FACE ( 'NONE', ( #5041 ), #15120, .T. ) ;
#246 = VERTEX_POINT ( 'NONE', #19148 ) ;
#245 = CARTESIAN_POINT ( 'NONE',  ( -1.290629128713961293, 29.97320584640673147, 5.204870533884474071 ) ) ;
#247 = CARTESIAN_POINT ( 'NONE',  ( -4.000000000000001776, 29.21874999877097068, 8.999999999999992895 ) ) ;
#248 = CARTESIAN_POINT ( 'NONE',  ( -2.899999999999996358, -8.999999999999992895, 25.00000000000000000 ) ) ;
#249 = AXIS2_PLACEMENT_3D ( 'NONE', #7329, #17401, #17148 ) ;
#250 = ORIENTED_EDGE ( 'NONE', *, *, #20339, .T. ) ;
#251 = CARTESIAN_POINT ( 'NONE',  ( 4.000000000000002665, 26.70624999877097849, 11.30940107675849760 ) ) ;
#252 = CARTESIAN_POINT ( 'NONE',  ( 13.69242354489153080, 27.92360179968372691, -6.500000000000000000 ) ) ;
#253 = CARTESIAN_POINT ( 'NONE',  ( 1.878215178124998497, -26.79062499938548214, 12.25316411605951927 ) ) ;
#255 = ORIENTED_EDGE ( 'NONE', *, *, #13059, .F. ) ;
#254 = DIRECTION ( 'NONE',  ( 0.000000000000000000, 0.000000000000000000, 1.000000000000000000 ) ) ;
#256 = VERTEX_POINT ( 'NONE', #11047 ) ;
#257 = ORIENTED_EDGE ( 'NONE', *, *, #741, .T. ) ;
#258 =( REPRESENTATION_RELATIONSHIP ('NONE','NONE', #25031, #22515 ) REPRESENTATION_RELATIONSHIP_WITH_TRANSFORMATION ( #10219 )SHAPE_REPRESENTATION_RELATIONSHIP( ) );
#259 = CIRCLE ( 'NONE', #6931, 0.4999999999999998335 ) ;
#260 = ORIENTED_EDGE ( 'NONE', *, *, #5301, .F. ) ;
#261 = CARTESIAN_POINT ( 'NONE',  ( -10.08469938919519926, -29.41953157733083302, -6.500000000000000000 ) ) ;
#262 = CARTESIAN_POINT ( 'NONE',  ( -3.999999999999997335, 27.00624999877096855, 11.30940107675849404 ) ) ;
#263 = CARTESIAN_POINT ( 'NONE',  ( 3.834746474454188013E-15, 26.40624999877096357, 4.999999999999992006 ) ) ;
#264 = CARTESIAN_POINT ( 'NONE',  ( 1.878215178125001605, 27.76562499938548711, 12.25316411605952283 ) ) ;
#265 = DIRECTION ( 'NONE',  ( -0.000000000000000000, 0.000000000000000000, 1.000000000000000000 ) ) ;
#266 = CARTESIAN_POINT ( 'NONE',  ( -1.999999999999995781, -5.535898384862237620, 4.593749998770966236 ) ) ;
#267 = CARTESIAN_POINT ( 'NONE',  ( -1.878215178124998497, 26.34062499938548285, 12.25316411605951927 ) ) ;
#268 = CARTESIAN_POINT ( 'NONE',  ( -29.57785765677917311, 9.610428525061202265, -6.500000000000000000 ) ) ;
#269 = LINE ( 'NONE', #15826, #13033 ) ;
#270 = ADVANCED_FACE ( 'NONE', ( #14589 ), #20734, .T. ) ;
#271 = CARTESIAN_POINT ( 'NONE',  ( -3.756430356249996994, 25.81562499938548427, 8.999999999999992895 ) ) ;
#272 = CARTESIAN_POINT ( 'NONE',  ( -23.96296185032681336, 19.82388608118453632, 1.000000000000000000 ) ) ;
#273 = CARTESIAN_POINT ( 'NONE',  ( -19.82388608118446527, -23.96296185032687376, -6.500000000000000000 ) ) ;
#274 = CARTESIAN_POINT ( 'NONE',  ( 15.32653948221845575, 20.98339373171076971, 8.999999999999992895 ) ) ;
#275 = CARTESIAN_POINT ( 'NONE',  ( 3.999999999999996003, -29.18124999877096926, 6.690598923241487306 ) ) ;
#276 = DIRECTION ( 'NONE',  ( 1.000000000000000000, 0.000000000000000000, 0.000000000000000000 ) ) ;
#277 = ADVANCED_FACE ( 'NONE', ( #3080 ), #9085, .T. ) ;
#278 = DIRECTION ( 'NONE',  ( 0.000000000000000000, 1.000000000000000000, 0.000000000000000000 ) ) ;
#279 = CARTESIAN_POINT ( 'NONE',  ( 3.999999999999994227, -11.30940107675849937, 1.762499999999997735 ) ) ;
#280 = CARTESIAN_POINT ( 'NONE',  ( 3.178742173564956808, -29.83148068024111410, 6.557713274934318548 ) ) ;
#281 = ORIENTED_EDGE ( 'NONE', *, *, #13641, .F. ) ;
#282 = CARTESIAN_POINT ( 'NONE',  ( 1.057460391440397258E-14, -29.16249999999999787, 4.999999999999992006 ) ) ;
#284 = VERTEX_POINT ( 'NONE', #18909 ) ;
#283 = FACE_OUTER_BOUND ( 'NONE', #1653, .T. ) ;
#285 = EDGE_LOOP ( 'NONE', ( #3996, #19961, #21885, #25596, #64, #22498, #18380, #2629, #2882, #13648, #16581, #11690, #2311, #3515, #5348, #18845, #16021, #25747, #20827, #6154, #13089, #936, #2532, #21309 ) ) ;
#286 = ORIENTED_EDGE ( 'NONE', *, *, #2780, .F. ) ;
#287 = ORIENTED_EDGE ( 'NONE', *, *, #24315, .F. ) ;
#288 = ORIENTED_EDGE ( 'NONE', *, *, #23099, .T. ) ;
#289 = CARTESIAN_POINT ( 'NONE',  ( 29.09636799667075024, -10.98232076577232519, -2.750000000000000000 ) ) ;
#290 = EDGE_LOOP ( 'NONE', ( #13571, #12401, #24240, #13980, #21957, #2916, #23588, #1468, #14108, #13538, #2496, #5234, #22275, #20569, #6506, #25331, #10531, #8615, #1170, #12139, #14587, #14625, #15332, #12330, #21832 ) ) ;
#291 = CARTESIAN_POINT ( 'NONE',  ( 2.620986760973688460E-15, 29.38749999999999929, 13.61880215351699874 ) ) ;
#292 = CARTESIAN_POINT ( 'NONE',  ( 3.756430356250002323, 27.01562499938548356, 11.16877607737301403 ) ) ;
#293 = CARTESIAN_POINT ( 'NONE',  ( -3.756430356249996994, -8.999999999999992895, 2.728124999385482585 ) ) ;
#294 = CARTESIAN_POINT ( 'NONE',  ( -1.999999999999995781, -5.535898384862237620, 1.443749998770966325 ) ) ;
#295 = CARTESIAN_POINT ( 'NONE',  ( 20.11283227250407180, 17.45663489454462436, 5.746835883940462963 ) ) ;
#296 = LINE ( 'NONE', #16630, #5040 ) ;
#297 = DIRECTION ( 'NONE',  ( 0.000000000000000000, -0.000000000000000000, 1.000000000000000000 ) ) ;
#298 = CARTESIAN_POINT ( 'NONE',  ( 1.878215178125000939, -12.25316411605952283, 0.9656249993854824076 ) ) ;
#299 = DIRECTION ( 'NONE',  ( 1.000000000000000000, 0.000000000000000000, 0.000000000000000000 ) ) ;
#300 = EDGE_CURVE ( 'NONE', #5668, #20971, #6231, .T. ) ;
#301 = CARTESIAN_POINT ( 'NONE',  ( 3.756430356250003655, 29.64062499938548356, 8.999999999999992895 ) ) ;
#302 = DIRECTION ( 'NONE',  ( 0.000000000000000000, 0.000000000000000000, -1.000000000000000000 ) ) ;
#303 = DIRECTION ( 'NONE',  ( 1.000000000000000000, 0.000000000000000000, 0.000000000000000000 ) ) ;
#304 = CARTESIAN_POINT ( 'NONE',  ( 21.21320343559646915, 21.21320343559638744, 8.999999999999992895 ) ) ;
#305 = ORIENTED_EDGE ( 'NONE', *, *, #21565, .F. ) ;
#306 = EDGE_LOOP ( 'NONE', ( #6770, #6578, #10344, #18560 ) ) ;
#307 = CARTESIAN_POINT ( 'NONE',  ( -3.756430356250002323, 27.31562499938548783, 11.16877607737301226 ) ) ;
#308 = EDGE_CURVE ( 'NONE', #5737, #11616, #8580, .T. ) ;
#309 = ORIENTED_EDGE ( 'NONE', *, *, #9443, .F. ) ;
#310 = DIRECTION ( 'NONE',  ( 0.000000000000000000, -0.000000000000000000, 1.000000000000000000 ) ) ;
#311 = VERTEX_POINT ( 'NONE', #18646 ) ;
#312 = CARTESIAN_POINT ( 'NONE',  ( 21.42091605170094937, 15.76406180220850040, 8.999999999999992895 ) ) ;
#313 = ORIENTED_EDGE ( 'NONE', *, *, #21775, .T. ) ;
#314 = EDGE_CURVE ( 'NONE', #21568, #311, #8696, .T. ) ;
#315 = DIRECTION ( 'NONE',  ( 0.000000000000000000, 1.000000000000000000, 0.000000000000000000 ) ) ;
#316 = ORIENTED_EDGE ( 'NONE', *, *, #23479, .F. ) ;
#317 = DIRECTION ( 'NONE',  ( -0.000000000000000000, -0.000000000000000000, 1.000000000000000000 ) ) ;
#318 = CARTESIAN_POINT ( 'NONE',  ( 2.672651547586948120E-15, 28.17812499938548143, 13.33755215474602984 ) ) ;
#319 = CARTESIAN_POINT ( 'NONE',  ( 4.000000000000003553, 29.08750000000000213, 6.690598923241489970 ) ) ;
#320 = DIRECTION ( 'NONE',  ( 0.000000000000000000, 0.000000000000000000, 1.000000000000000000 ) ) ;
#321 = FACE_OUTER_BOUND ( 'NONE', #5229, .T. ) ;
#322 = CARTESIAN_POINT ( 'NONE',  ( -3.999999999999996447, 28.86250000000000071, 11.30940107675849404 ) ) ;
#323 = CARTESIAN_POINT ( 'NONE',  ( -3.756430356249995661, 26.67812499938548498, 6.831223922626973533 ) ) ;
#324 = DIRECTION ( 'NONE',  ( 0.000000000000000000, 0.000000000000000000, 1.000000000000000000 ) ) ;
#325 = CARTESIAN_POINT ( 'NONE',  ( 18.91510639674018890, 21.74353352148630236, 5.535898384862237620 ) ) ;
#326 = CYLINDRICAL_SURFACE ( 'NONE', #16421, 0.5000000000000004441 ) ;
#327 = DIRECTION ( 'NONE',  ( -0.000000000000000000, -0.000000000000000000, 1.000000000000000000 ) ) ;
#328 = CARTESIAN_POINT ( 'NONE',  ( 4.000000000000003553, 25.03750000000000142, 6.690598923241489970 ) ) ;
#329 = CARTESIAN_POINT ( 'NONE',  ( 1.878215178124998497, -25.89062499938548356, 12.25316411605951927 ) ) ;
#330 = EDGE_CURVE ( 'NONE', #22681, #23712, #2540, .T. ) ;
#331 = AXIS2_PLACEMENT_3D ( 'NONE', #1726, #17803, #5513 ) ;
#332 = CARTESIAN_POINT ( 'NONE',  ( 0.000000000000000000, 0.000000000000000000, -6.500000000000000000 ) ) ;
#333 = ORIENTED_EDGE ( 'NONE', *, *, #23959, .T. ) ;
#334 = CARTESIAN_POINT ( 'NONE',  ( -1.999999999999998224, 26.59374999877096712, 12.46410161513774639 ) ) ;
#335 = CARTESIAN_POINT ( 'NONE',  ( 0.000000000000000000, 0.000000000000000000, 20.00000000000000000 ) ) ;
#337 = VERTEX_POINT ( 'NONE', #16684 ) ;
#336 = CARTESIAN_POINT ( 'NONE',  ( -1.878215178124998275, 28.25312499938548783, 12.25316411605951927 ) ) ;
#338 = ORIENTED_EDGE ( 'NONE', *, *, #8418, .T. ) ;
#339 = CARTESIAN_POINT ( 'NONE',  ( 1.071796769724493448, -29.12634618820329990, 4.999999999999995559 ) ) ;
#340 = EDGE_CURVE ( 'NONE', #19215, #8133, #14856, .T. ) ;
#341 = LINE ( 'NONE', #20331, #16761 ) ;
#342 = CARTESIAN_POINT ( 'NONE',  ( -1.999999999999998224, 25.69374999877097210, 12.46410161513774639 ) ) ;
#343 = AXIS2_PLACEMENT_3D ( 'NONE', #22234, #14397, #10312 ) ;
#344 = EDGE_CURVE ( 'NONE', #1313, #21005, #7390, .T. ) ;
#345 = VERTEX_POINT ( 'NONE', #10775 ) ;
#346 = ORIENTED_EDGE ( 'NONE', *, *, #25545, .F. ) ;
#347 = CARTESIAN_POINT ( 'NONE',  ( 3.756430356249996994, -26.82812499938548711, 8.999999999999992895 ) ) ;
#348 = CARTESIAN_POINT ( 'NONE',  ( -1.878215178124999829, 29.04062499938549280, 12.25316411605951927 ) ) ;
#349 = DIRECTION ( 'NONE',  ( -0.000000000000000000, -0.000000000000000000, 1.000000000000000000 ) ) ;
#350 = CARTESIAN_POINT ( 'NONE',  ( 1.878215178125000939, -12.25316411605952283, 4.565624999385481608 ) ) ;
#351 = ADVANCED_FACE ( 'NONE', ( #18768 ), #8839, .F. ) ;
#352 = CIRCLE ( 'NONE', #6610, 6.000000000000000000 ) ;
#353 = CARTESIAN_POINT ( 'NONE',  ( 3.752267015613588906E-15, -4.381197846482986158, 1.012499999999998401 ) ) ;
#354 = CARTESIAN_POINT ( 'NONE',  ( 18.68225429291731743, 24.86329371854767700, -2.750000000000000000 ) ) ;
#355 = AXIS2_PLACEMENT_3D ( 'NONE', #19379, #17425, #11406 ) ;
#356 = CARTESIAN_POINT ( 'NONE',  ( 19.96824085905927149, 21.48399038691124474, 12.99999999999999289 ) ) ;
#357 = CARTESIAN_POINT ( 'NONE',  ( 0.000000000000000000, 0.000000000000000000, 0.000000000000000000 ) ) ;
#358 = CIRCLE ( 'NONE', #25835, 0.5000000000000001110 ) ;
#359 = CARTESIAN_POINT ( 'NONE',  ( -28.41604871112473418, -11.44867358849319849, 1.000000000000000000 ) ) ;
#360 = CARTESIAN_POINT ( 'NONE',  ( -3.469446951953614189E-15, -30.00000000000000355, 8.999999999999992895 ) ) ;
#362 = EDGE_CURVE ( 'NONE', #3397, #1343, #25563, .T. ) ;
#361 = CARTESIAN_POINT ( 'NONE',  ( 21.67957950013421353, 16.36718474421539682, 11.16877607737301226 ) ) ;
#363 = CARTESIAN_POINT ( 'NONE',  ( 16.55955693104344206, 22.21641118053575426, 8.999999999999992895 ) ) ;
#364 = VERTEX_POINT ( 'NONE', #23208 ) ;
#365 = CARTESIAN_POINT ( 'NONE',  ( 3.999999999999996447, -27.02500000000000213, 8.999999999999992895 ) ) ;
#366 = CYLINDRICAL_SURFACE ( 'NONE', #12999, 31.10000000000000142 ) ;
#367 = CARTESIAN_POINT ( 'NONE',  ( -1.878215178124995832, 26.19062499938548427, 5.746835883940462963 ) ) ;
#369 = ORIENTED_EDGE ( 'NONE', *, *, #4197, .F. ) ;
#368 = CARTESIAN_POINT ( 'NONE',  ( -2.007411586324088226, 29.93355017142139118, 12.46960170373642640 ) ) ;
#370 = CARTESIAN_POINT ( 'NONE',  ( 17.85665593321704137, 17.85665593321697386, 4.662447845253954171 ) ) ;
#371 = CARTESIAN_POINT ( 'NONE',  ( -1.626862140677534194E-14, -28.03750000000000497, 12.99999999999999289 ) ) ;
#372 = ORIENTED_EDGE ( 'NONE', *, *, #5336, .T. ) ;
#373 = CARTESIAN_POINT ( 'NONE',  ( 0.5000000000000001110, 6.123233995736767268E-17, 19.50000000000000000 ) ) ;
#374 = CARTESIAN_POINT ( 'NONE',  ( 2.620986760973688460E-15, 26.63124999877097565, 13.61880215351699874 ) ) ;
#375 = CARTESIAN_POINT ( 'NONE',  ( 3.756430356249996994, -26.71562499938548285, 8.999999999999992895 ) ) ;
#377 = ORIENTED_EDGE ( 'NONE', *, *, #20034, .T. ) ;
#376 = CARTESIAN_POINT ( 'NONE',  ( 0.000000000000000000, 0.000000000000000000, 1.000000000000000000 ) ) ;
#378 =( BOUNDED_SURFACE ( )  B_SPLINE_SURFACE ( 1, 2, ( 
 ( #13327, #4838, #19341, #20924, #22880, #1434, #9406, #21174, #3135, #17002, #12814, #4962, #7189, #20786, #15037, #25350, #2867, #13081, #11220, #6925, #23017, #1299, #25102, #18831, #16884, #24849, #12943, #3008, #5102, #19080, #21056, #1160, #9139, #17891, #17645, #21682, #17504, #1943, #3518, #25864, #15939, #3767, #9522, #1554, #21822, #11746, #11489, #120, #9906, #11875, #9662, #25615, #7952, #19726, #15556, #25482, #1823, #13976, #7819, #7568, #11990, #23525, #23911, #18034, #23770, #5859, #13843, #1686, #8091, #3904, #15800, #5992, #19842, #7699, #19964, #5609, #21945, #4023, #2068, #10036, #9787, #23392, #17767, #13589, #15680, #5476, #25736, #5725, #13471, #21437, #19462, #21556, #3636, #11608, #19582, #23648, #13706, #4676, #10672, #22594, #20627, #12655, #2710, #10549, #12262, #18662, #18165, #2327, #20231, #18548, #10286, #12513, #6115, #4291, #16325, #4150, #2586, #22063, #16070, #16187, #243 ),
 ( #505, #8213, #8475, #749, #24153, #16461, #2208, #24033, #14098, #10408, #6244, #16579, #12128, #20104, #10167, #6623, #24538, #22329, #24294, #4411, #14234, #22204, #6379, #18279, #24423, #2447, #6500, #14485, #367, #18407, #8337, #14369, #12385, #20489, #14613, #22452, #20351, #4533, #630, #8597, #3101, #21023, #1013, #4808, #24934, #3347, #8990, #10801, #2833, #13173, #6764, #9102, #21142, #19168, #11184, #25065, #3214, #24678, #11067, #13290, #19045, #17092, #881, #7284, #12783, #20755, #14750, #16967, #18793, #22728, #8864, #1261, #21266, #1128, #16850, #25206, #24814, #7153, #4924, #14875, #23112, #9246, #15143, #15261, #17234, #15000, #12908, #19305, #23229, #5312, #6892, #5194, #11323, #8718, #16705, #2972, #13044, #22850, #20884, #10939, #18930, #7013, #22979, #5065, #21911, #5441, #15767, #13673, #23733, #21644, #9623, #15523, #23491, #23352, #3727, #7401, #9756, #17735, #19429, #3604, #1402 ) ),
 .UNSPECIFIED., .F., .F., .F. ) 
 B_SPLINE_SURFACE_WITH_KNOTS ( ( 2, 2 ),
 ( 3, 2, 2, 2, 2, 2, 2, 2, 2, 2, 2, 2, 2, 2, 2, 2, 2, 2, 2, 2, 2, 2, 2, 2, 2, 2, 2, 2, 2, 2, 2, 2, 2, 2, 2, 2, 2, 2, 2, 2, 2, 2, 2, 2, 2, 2, 2, 2, 2, 2, 2, 2, 2, 2, 2, 2, 2, 2, 2, 2, 3 ),
 ( 0.000000000000000000, 1.000000000000000000 ),
 ( 0.000000000000000000, 0.01666666666666666644, 0.03333333333333333287, 0.05000000000000000278, 0.06666666666666666574, 0.08333333333333332871, 0.1000000000000000056, 0.1166666666666666685, 0.1333333333333333315, 0.1499999999999999944, 0.1666666666666666574, 0.1833333333333333204, 0.2000000000000000111, 0.2166666666666666741, 0.2333333333333333370, 0.2500000000000000000, 0.2666666666666666630, 0.2833333333333333259, 0.2999999999999999889, 0.3166666666666666519, 0.3333333333333333148, 0.3499999999999999778, 0.3666666666666666408, 0.3833333333333333592, 0.4000000000000000222, 0.4166666666666666852, 0.4333333333333333481, 0.4500000000000000111, 0.4666666666666666741, 0.4833333333333333370, 0.5000000000000000000, 0.5166666666666667185, 0.5333333333333333259, 0.5500000000000000444, 0.5666666666666666519, 0.5833333333333333703, 0.5999999999999999778, 0.6166666666666666963, 0.6333333333333333037, 0.6500000000000000222, 0.6666666666666666297, 0.6833333333333333481, 0.6999999999999999556, 0.7166666666666666741, 0.7333333333333332815, 0.7500000000000000000, 0.7666666666666667185, 0.7833333333333333259, 0.8000000000000000444, 0.8166666666666666519, 0.8333333333333333703, 0.8499999999999999778, 0.8666666666666666963, 0.8833333333333333037, 0.9000000000000000222, 0.9166666666666666297, 0.9333333333333333481, 0.9499999999999999556, 0.9666666666666666741, 0.9833333333333332815, 1.000000000000000000 ),
 .UNSPECIFIED. ) 
 GEOMETRIC_REPRESENTATION_ITEM ( )  RATIONAL_B_SPLINE_SURFACE ( (
 ( 1.000000000000000000, 0.8660254037844387076, 1.000000000000000000, 0.8660254037844387076, 1.000000000000000000, 0.8660254037844387076, 1.000000000000000000, 0.8660254037844387076, 1.000000000000000000, 0.8660254037844387076, 1.000000000000000000, 0.8660254037844387076, 1.000000000000000000, 0.8660254037844387076, 1.000000000000000000, 0.8660254037844387076, 1.000000000000000000, 0.8660254037844387076, 1.000000000000000000, 0.8660254037844387076, 1.000000000000000000, 0.8660254037844387076, 1.000000000000000000, 0.8660254037844387076, 1.000000000000000000, 0.8660254037844387076, 1.000000000000000000, 0.8660254037844387076, 1.000000000000000000, 0.8660254037844387076, 1.000000000000000000, 0.8660254037844387076, 1.000000000000000000, 0.8660254037844387076, 1.000000000000000000, 0.8660254037844387076, 1.000000000000000000, 0.8660254037844387076, 1.000000000000000000, 0.8660254037844387076, 1.000000000000000000, 0.8660254037844387076, 1.000000000000000000, 0.8660254037844387076, 1.000000000000000000, 0.8660254037844387076, 1.000000000000000000, 0.8660254037844387076, 1.000000000000000000, 0.8660254037844387076, 1.000000000000000000, 0.8660254037844387076, 1.000000000000000000, 0.8660254037844387076, 1.000000000000000000, 0.8660254037844387076, 1.000000000000000000, 0.8660254037844387076, 1.000000000000000000, 0.8660254037844387076, 1.000000000000000000, 0.8660254037844387076, 1.000000000000000000, 0.8660254037844387076, 1.000000000000000000, 0.8660254037844387076, 1.000000000000000000, 0.8660254037844387076, 1.000000000000000000, 0.8660254037844387076, 1.000000000000000000, 0.8660254037844387076, 1.000000000000000000, 0.8660254037844387076, 1.000000000000000000, 0.8660254037844387076, 1.000000000000000000, 0.8660254037844387076, 1.000000000000000000, 0.8660254037844387076, 1.000000000000000000, 0.8660254037844387076, 1.000000000000000000, 0.8660254037844387076, 1.000000000000000000, 0.8660254037844387076, 1.000000000000000000, 0.8660254037844387076, 1.000000000000000000, 0.8660254037844387076, 1.000000000000000000, 0.8660254037844387076, 1.000000000000000000, 0.8660254037844387076, 1.000000000000000000, 0.8660254037844387076, 1.000000000000000000, 0.8660254037844387076, 1.000000000000000000, 0.8660254037844387076, 1.000000000000000000, 0.8660254037844387076, 1.000000000000000000, 0.8660254037844387076, 1.000000000000000000, 0.8660254037844387076, 1.000000000000000000, 0.8660254037844387076, 1.000000000000000000, 0.8660254037844387076, 1.000000000000000000, 0.8660254037844387076, 1.000000000000000000, 0.8660254037844387076, 1.000000000000000000, 0.8660254037844387076, 1.000000000000000000, 0.8660254037844387076, 1.000000000000000000, 0.8660254037844387076, 1.000000000000000000),
 ( 1.000000000000000000, 0.8660254037844387076, 1.000000000000000000, 0.8660254037844387076, 1.000000000000000000, 0.8660254037844387076, 1.000000000000000000, 0.8660254037844387076, 1.000000000000000000, 0.8660254037844387076, 1.000000000000000000, 0.8660254037844387076, 1.000000000000000000, 0.8660254037844387076, 1.000000000000000000, 0.8660254037844387076, 1.000000000000000000, 0.8660254037844387076, 1.000000000000000000, 0.8660254037844387076, 1.000000000000000000, 0.8660254037844387076, 1.000000000000000000, 0.8660254037844387076, 1.000000000000000000, 0.8660254037844387076, 1.000000000000000000, 0.8660254037844387076, 1.000000000000000000, 0.8660254037844387076, 1.000000000000000000, 0.8660254037844387076, 1.000000000000000000, 0.8660254037844387076, 1.000000000000000000, 0.8660254037844387076, 1.000000000000000000, 0.8660254037844387076, 1.000000000000000000, 0.8660254037844387076, 1.000000000000000000, 0.8660254037844387076, 1.000000000000000000, 0.8660254037844387076, 1.000000000000000000, 0.8660254037844387076, 1.000000000000000000, 0.8660254037844387076, 1.000000000000000000, 0.8660254037844387076, 1.000000000000000000, 0.8660254037844387076, 1.000000000000000000, 0.8660254037844387076, 1.000000000000000000, 0.8660254037844387076, 1.000000000000000000, 0.8660254037844387076, 1.000000000000000000, 0.8660254037844387076, 1.000000000000000000, 0.8660254037844387076, 1.000000000000000000, 0.8660254037844387076, 1.000000000000000000, 0.8660254037844387076, 1.000000000000000000, 0.8660254037844387076, 1.000000000000000000, 0.8660254037844387076, 1.000000000000000000, 0.8660254037844387076, 1.000000000000000000, 0.8660254037844387076, 1.000000000000000000, 0.8660254037844387076, 1.000000000000000000, 0.8660254037844387076, 1.000000000000000000, 0.8660254037844387076, 1.000000000000000000, 0.8660254037844387076, 1.000000000000000000, 0.8660254037844387076, 1.000000000000000000, 0.8660254037844387076, 1.000000000000000000, 0.8660254037844387076, 1.000000000000000000, 0.8660254037844387076, 1.000000000000000000, 0.8660254037844387076, 1.000000000000000000, 0.8660254037844387076, 1.000000000000000000, 0.8660254037844387076, 1.000000000000000000, 0.8660254037844387076, 1.000000000000000000, 0.8660254037844387076, 1.000000000000000000, 0.8660254037844387076, 1.000000000000000000, 0.8660254037844387076, 1.000000000000000000, 0.8660254037844387076, 1.000000000000000000, 0.8660254037844387076, 1.000000000000000000, 0.8660254037844387076, 1.000000000000000000, 0.8660254037844387076, 1.000000000000000000, 0.8660254037844387076, 1.000000000000000000, 0.8660254037844387076, 1.000000000000000000, 0.8660254037844387076, 1.000000000000000000, 0.8660254037844387076, 1.000000000000000000) ) ) 
 REPRESENTATION_ITEM ( '' )  SURFACE ( )  );
#379 = AXIS2_PLACEMENT_3D ( 'NONE', #21267, #11325, #1788 ) ;
#380 = VERTEX_POINT ( 'NONE', #21626 ) ;
#381 = EDGE_LOOP ( 'NONE', ( #3819, #17426, #15116, #9054 ) ) ;
#382 = AXIS2_PLACEMENT_3D ( 'NONE', #14480, #16700, #6759 ) ;
#383 = VERTEX_POINT ( 'NONE', #19283 ) ;
#384 = ADVANCED_FACE ( 'NONE', ( #5558 ), #46, .T. ) ;
#385 = PLANE ( 'NONE',  #17255 ) ;
#386 = CARTESIAN_POINT ( 'NONE',  ( -1.878215178124998275, 25.55312499938549564, 12.25316411605951927 ) ) ;
#387 = CIRCLE ( 'NONE', #2056, 31.10000000000000142 ) ;
#388 = AXIS2_PLACEMENT_3D ( 'NONE', #11786, #19763, #1858 ) ;
#389 = EDGE_CURVE ( 'NONE', #6543, #18698, #23590, .T. ) ;
#390 = EDGE_CURVE ( 'NONE', #22273, #20492, #21386, .T. ) ;
#391 = DIRECTION ( 'NONE',  ( 0.000000000000000000, 0.000000000000000000, -1.000000000000000000 ) ) ;
#392 = CARTESIAN_POINT ( 'NONE',  ( 3.735045420075836212E-15, -4.662447845253954171, 2.165624999385483029 ) ) ;
#393 = CARTESIAN_POINT ( 'NONE',  ( -3.756430356249995661, 26.67812499938548498, 6.831223922626973533 ) ) ;
#394 = CARTESIAN_POINT ( 'NONE',  ( 15.41874213889396117, -27.00874656207311020, 1.000000000000000000 ) ) ;
#395 = AXIS2_PLACEMENT_3D ( 'NONE', #11615, #6002, #7707 ) ;
#396 = CARTESIAN_POINT ( 'NONE',  ( 0.000000000000000000, 31.10000000000000142, -6.500000000000000000 ) ) ;
#397 = CARTESIAN_POINT ( 'NONE',  ( -3.756430356249996105, 25.77812499938548285, 6.831223922626973533 ) ) ;
#398 = CARTESIAN_POINT ( 'NONE',  ( 3.918623196469464443, 31.50000000000000000, 4.456389954662531849 ) ) ;
#399 = DIRECTION ( 'NONE',  ( 1.000000000000000000, 0.000000000000000000, 0.000000000000000000 ) ) ;
#400 = CARTESIAN_POINT ( 'NONE',  ( -1.999999999999995781, 28.69374999877096855, 5.535898384862237620 ) ) ;
#401 = CARTESIAN_POINT ( 'NONE',  ( -3.756430356250003655, -25.70312499938548356, 8.999999999999992895 ) ) ;
#402 = FACE_OUTER_BOUND ( 'NONE', #9294, .T. ) ;
#403 = AXIS2_PLACEMENT_3D ( 'NONE', #22410, #18239, #9988 ) ;
#404 = CARTESIAN_POINT ( 'NONE',  ( 4.000000000000003553, -8.999999999999992895, 2.700000000000001066 ) ) ;
#406 = LINE ( 'NONE', #6283, #17518 ) ;
#405 = AXIS2_PLACEMENT_3D ( 'NONE', #13535, #2006, #15875 ) ;
#407 = CARTESIAN_POINT ( 'NONE',  ( -22.17092431280563503, 21.28941499438250062, -6.500000000000000000 ) ) ;
#408 = VERTEX_POINT ( 'NONE', #21244 ) ;
#409 = CARTESIAN_POINT ( 'NONE',  ( 2.000000000000003553, 27.71874999877097778, 5.535898384862238508 ) ) ;
#411 = ORIENTED_EDGE ( 'NONE', *, *, #12740, .F. ) ;
#410 = CARTESIAN_POINT ( 'NONE',  ( 21.21320343559646915, 21.21320343559638744, 8.999999999999992895 ) ) ;
#412 = ORIENTED_EDGE ( 'NONE', *, *, #15667, .F. ) ;
#413 = CIRCLE ( 'NONE', #7088, 1.500000000000000222 ) ;
#414 = VERTEX_POINT ( 'NONE', #11303 ) ;
#415 = EDGE_LOOP ( 'NONE', ( #19879, #25527, #12734, #3697 ) ) ;
#416 = ORIENTED_EDGE ( 'NONE', *, *, #10693, .T. ) ;
#417 = ORIENTED_EDGE ( 'NONE', *, *, #13846, .T. ) ;
#418 = FACE_OUTER_BOUND ( 'NONE', #25244, .T. ) ;
#419 = CIRCLE ( 'NONE', #13349, 31.10000000000000142 ) ;
#420 = AXIS2_PLACEMENT_3D ( 'NONE', #4845, #24723, #6933 ) ;
#421 = VERTEX_POINT ( 'NONE', #17718 ) ;
#422 = EDGE_CURVE ( 'NONE', #16170, #9403, #21906, .T. ) ;
#423 = LINE ( 'NONE', #3954, #1333 ) ;
#424 = CARTESIAN_POINT ( 'NONE',  ( -1.878215178124995832, 25.85312499938548569, 5.746835883940462963 ) ) ;
#426 = ADVANCED_FACE ( 'NONE', ( #15751 ), #3586, .T. ) ;
#425 = AXIS2_PLACEMENT_3D ( 'NONE', #20340, #2434, #1117 ) ;
#427 = AXIS2_PLACEMENT_3D ( 'NONE', #1473, #13891, #21596 ) ;
#428 = CARTESIAN_POINT ( 'NONE',  ( 3.756430356250002323, -11.16877607737301226, 1.565624999385482941 ) ) ;
#429 = CARTESIAN_POINT ( 'NONE',  ( -4.000000000000033751, -6.690598923241509510, 1.481249998770963749 ) ) ;
#430 = CARTESIAN_POINT ( 'NONE',  ( 20.64316235839397962, 17.98696498043453573, 12.25316411605952283 ) ) ;
#431 = EDGE_CURVE ( 'NONE', #13647, #11427, #23332, .T. ) ;
#432 = DIRECTION ( 'NONE',  ( -0.000000000000000000, -0.000000000000000000, 1.000000000000000000 ) ) ;
#433 = AXIS2_PLACEMENT_3D ( 'NONE', #24646, #6868, #8833 ) ;
#434 = CARTESIAN_POINT ( 'NONE',  ( 1.878215178125004048, -5.746835883940462963, 1.565624999385482274 ) ) ;
#435 = CARTESIAN_POINT ( 'NONE',  ( 2.000000000000003997, -5.535898384862238508, 3.675000000000001155 ) ) ;
#436 = LINE ( 'NONE', #14425, #4662 ) ;
#437 = CARTESIAN_POINT ( 'NONE',  ( -1.878215178124995832, 28.89062499938548356, 5.746835883940462963 ) ) ;
#438 = CIRCLE ( 'NONE', #9607, 0.4999999999999996114 ) ;
#439 = CARTESIAN_POINT ( 'NONE',  ( -1.878215178124998497, -12.25316411605951927, 1.003124999385485161 ) ) ;
#440 = CARTESIAN_POINT ( 'NONE',  ( 18.19474136253732865, 18.19474136253726826, 12.99999999999999289 ) ) ;
#441 = VECTOR ( 'NONE', #4538, 1000.000000000000000 ) ;
#442 = CARTESIAN_POINT ( 'NONE',  ( -3.897863563849436552, 30.85476721088031482, -6.500000000000000000 ) ) ;
#443 = ORIENTED_EDGE ( 'NONE', *, *, #15873, .T. ) ;
#444 = ORIENTED_EDGE ( 'NONE', *, *, #3058, .F. ) ;
#445 = CARTESIAN_POINT ( 'NONE',  ( -1.878215178124994722, 26.75312499938549138, 5.746835883940462963 ) ) ;
#446 = VERTEX_POINT ( 'NONE', #13409 ) ;
#447 = LINE ( 'NONE', #10230, #15448 ) ;
#448 = EDGE_LOOP ( 'NONE', ( #16828, #9714, #24335, #4332 ) ) ;
#449 = CARTESIAN_POINT ( 'NONE',  ( -3.999999999999996447, 26.12500000000000355, 8.999999999999992895 ) ) ;
#450 = ORIENTED_EDGE ( 'NONE', *, *, #18741, .F. ) ;
#451 = DIRECTION ( 'NONE',  ( 0.7705132427757999114, 0.6374239897486768669, 0.000000000000000000 ) ) ;
#452 = CARTESIAN_POINT ( 'NONE',  ( -31.03863125411922752, 1.952785157361987878, -6.500000000000000000 ) ) ;
#453 = AXIS2_PLACEMENT_3D ( 'NONE', #20208, #10264, #5925 ) ;
#454 = ORIENTED_EDGE ( 'NONE', *, *, #18989, .T. ) ;
#455 = DIRECTION ( 'NONE',  ( 1.000000000000000000, 0.000000000000000000, 0.000000000000000000 ) ) ;
#456 = ADVANCED_FACE ( 'NONE', ( #9600 ), #3466, .T. ) ;
#457 = CARTESIAN_POINT ( 'NONE',  ( 2.672651547586948120E-15, 27.27812499938548285, 13.33755215474602984 ) ) ;
#458 = CARTESIAN_POINT ( 'NONE',  ( 3.469446951953614189E-15, 39.50000000000000000, 8.999999999999992895 ) ) ;
#459 =( GEOMETRIC_REPRESENTATION_CONTEXT ( 3 ) GLOBAL_UNCERTAINTY_ASSIGNED_CONTEXT ( ( #10970 ) ) GLOBAL_UNIT_ASSIGNED_CONTEXT ( ( #23012, #3129, #18575 ) ) REPRESENTATION_CONTEXT ( 'NONE', 'WORKASPACE' ) );
#460 = EDGE_CURVE ( 'NONE', #51, #5651, #19861, .T. ) ;
#461 = AXIS2_PLACEMENT_3D ( 'NONE', #21744, #5539, #19508 ) ;
#462 = LINE ( 'NONE', #12609, #10063 ) ;
#463 = DIRECTION ( 'NONE',  ( -0.000000000000000000, -1.000000000000000000, -0.000000000000000000 ) ) ;
#464 = DIRECTION ( 'NONE',  ( -0.000000000000000000, -0.000000000000000000, 1.000000000000000000 ) ) ;
#465 = CARTESIAN_POINT ( 'NONE',  ( 3.735045420075836212E-15, 27.05312499938548498, 4.662447845253954171 ) ) ;
#466 = EDGE_CURVE ( 'NONE', #13776, #14884, #16423, .T. ) ;
#467 = CARTESIAN_POINT ( 'NONE',  ( 17.93620544610053003, 17.93620544610046252, 4.662447845253954171 ) ) ;
#468 = CARTESIAN_POINT ( 'NONE',  ( 23.66156066545488201, 18.00470641596242771, 11.30940107675849760 ) ) ;
#469 = PRODUCT_DEFINITION_SHAPE ( 'NONE', 'NONE',  #20341 ) ;
#470 = CARTESIAN_POINT ( 'NONE',  ( 4.000000000000003553, -8.999999999999992895, 0.1968749993854837510 ) ) ;
#471 = CARTESIAN_POINT ( 'NONE',  ( 0.000000000000000000, 0.000000000000000000, 20.00001200000000168 ) ) ;
#472 = VECTOR ( 'NONE', #23351, 1000.000000000000000 ) ;
#473 = CARTESIAN_POINT ( 'NONE',  ( 3.369928719974892281E-15, 25.11250000000000426, 4.999999999999992006 ) ) ;
#474 = CIRCLE ( 'NONE', #15093, 0.4999999999999989453 ) ;
#475 = CARTESIAN_POINT ( 'NONE',  ( 5.255164635687713748, 38.99989214654019065, 10.62496012790605704 ) ) ;
#476 = VERTEX_POINT ( 'NONE', #17452 ) ;
#477 = CARTESIAN_POINT ( 'NONE',  ( -3.756430356249995661, 25.44062499938548427, 6.831223922626973533 ) ) ;
#478 = CARTESIAN_POINT ( 'NONE',  ( -4.000000000000003553, -28.15000000000000213, 8.999999999999992895 ) ) ;
#480 = ORIENTED_EDGE ( 'NONE', *, *, #22688, .F. ) ;
#479 = CARTESIAN_POINT ( 'NONE',  ( -1.878215178124998275, 28.10312499938548925, 5.746835883940462963 ) ) ;
#481 = ORIENTED_EDGE ( 'NONE', *, *, #22170, .T. ) ;
#482 = CARTESIAN_POINT ( 'NONE',  ( 3.469446951953614189E-15, 39.50000000000000000, 8.999999999999992895 ) ) ;
#483 = CIRCLE ( 'NONE', #7586, 0.4999999999999987232 ) ;
#484 = DIRECTION ( 'NONE',  ( -0.9685831611286283005, 0.2486898871648657861, 0.000000000000000000 ) ) ;
#485 = VERTEX_POINT ( 'NONE', #25421 ) ;
#486 = VERTEX_POINT ( 'NONE', #5677 ) ;
#487 = CARTESIAN_POINT ( 'NONE',  ( -1.878215178125004048, -27.57812499938548711, 5.746835883940462963 ) ) ;
#488 = CARTESIAN_POINT ( 'NONE',  ( 1.878215178125003382, 28.36562499938548498, 5.746835883940462963 ) ) ;
#489 = FACE_OUTER_BOUND ( 'NONE', #1615, .T. ) ;
#490 = CYLINDRICAL_SURFACE ( 'NONE', #24782, 0.5000000000000004441 ) ;
#491 = AXIS2_PLACEMENT_3D ( 'NONE', #8684, #8567, #22819 ) ;
#492 = CIRCLE ( 'NONE', #3822, 0.5000000000000004441 ) ;
#493 = ADVANCED_FACE ( 'NONE', ( #21765 ), #11688, .F. ) ;
#494 = CARTESIAN_POINT ( 'NONE',  ( 21.86285778994254514, 19.03443066519628601, 12.46410161513774817 ) ) ;
#495 = DIRECTION ( 'NONE',  ( -1.000000000000000000, 0.000000000000000000, 0.000000000000000000 ) ) ;
#496 = PLANE ( 'NONE',  #9182 ) ;
#497 = VECTOR ( 'NONE', #179, 1000.000000000000000 ) ;
#498 = DIRECTION ( 'NONE',  ( 1.000000000000000000, 0.000000000000000000, 0.000000000000000000 ) ) ;
#499 = CARTESIAN_POINT ( 'NONE',  ( 18.02680350200553150, 20.85523062675164851, 12.46410161513774639 ) ) ;
#500 = CARTESIAN_POINT ( 'NONE',  ( -10.08469938919507847, -29.41953157733087565, 1.000000000000000000 ) ) ;
#501 = CARTESIAN_POINT ( 'NONE',  ( 15.94292067550354730, 21.25531543142222901, 11.16877607737301226 ) ) ;
#502 = CARTESIAN_POINT ( 'NONE',  ( 22.18105584147648912, 19.35262871673023000, 12.46410161513774817 ) ) ;
#503 = CARTESIAN_POINT ( 'NONE',  ( 3.834746474454188013E-15, 28.26249999999999929, 4.999999999999992006 ) ) ;
#504 = CARTESIAN_POINT ( 'NONE',  ( 21.55218544786934132, 20.03643592001721530, 12.99999999999999467 ) ) ;
#505 = CARTESIAN_POINT ( 'NONE',  ( 3.756430356250003655, 25.14062499938548356, 8.999999999999992895 ) ) ;
#507 = ORIENTED_EDGE ( 'NONE', *, *, #9146, .T. ) ;
#506 = CARTESIAN_POINT ( 'NONE',  ( 27.09999999999999787, 0.6000000000000000888, 19.59999999999999787 ) ) ;
#508 = AXIS2_PLACEMENT_3D ( 'NONE', #23574, #21601, #11656 ) ;
#509 = CARTESIAN_POINT ( 'NONE',  ( 18.33395301051795911, 18.33395301051789517, 13.33755215474603162 ) ) ;
#510 = EDGE_LOOP ( 'NONE', ( #14113, #25279, #16262, #2593 ) ) ;
#511 = CARTESIAN_POINT ( 'NONE',  ( 3.756430356250003655, 29.69687499938548569, 8.999999999999992895 ) ) ;
#512 = LINE ( 'NONE', #2595, #15256 ) ;
#513 = CARTESIAN_POINT ( 'NONE',  ( 3.756430356249996994, -27.16562499938548214, 8.999999999999992895 ) ) ;
#515 = ORIENTED_EDGE ( 'NONE', *, *, #15269, .F. ) ;
#514 = CARTESIAN_POINT ( 'NONE',  ( -3.999999999999995559, 25.18750000000000000, 6.690598923241487306 ) ) ;
#516 = AXIS2_PLACEMENT_3D ( 'NONE', #10572, #16873, #22870 ) ;
#517 = LINE ( 'NONE', #10811, #790 ) ;
#518 = AXIS2_PLACEMENT_3D ( 'NONE', #19501, #15217, #9328 ) ;
#519 = ORIENTED_EDGE ( 'NONE', *, *, #19200, .F. ) ;
#520 = CARTESIAN_POINT ( 'NONE',  ( 3.756430356249995661, -29.49062499938548498, 6.831223922626973533 ) ) ;
#521 = ORIENTED_EDGE ( 'NONE', *, *, #2339, .F. ) ;
#522 = AXIS2_PLACEMENT_3D ( 'NONE', #18913, #11050, #20738 ) ;
#523 = VERTEX_POINT ( 'NONE', #23469 ) ;
#524 = CARTESIAN_POINT ( 'NONE',  ( 1.487416814333745711E-14, 28.03750000000001208, 12.99999999999999289 ) ) ;
#525 = CARTESIAN_POINT ( 'NONE',  ( 1.878215178125005158, 25.77812499938548996, 5.746835883940462963 ) ) ;
#526 = CARTESIAN_POINT ( 'NONE',  ( -1.999999999999995781, -5.535898384862237620, 1.950000000000000400 ) ) ;
#527 = CIRCLE ( 'NONE', #22224, 31.10000000000000142 ) ;
#528 = CARTESIAN_POINT ( 'NONE',  ( -3.756430356249997882, -11.16877607737301226, 3.215624999385481964 ) ) ;
#529 = SURFACE_STYLE_FILL_AREA ( #10305 ) ;
#530 = CARTESIAN_POINT ( 'NONE',  ( -3.481870629348635671, 38.92501902593045315, 4.645898033751316270 ) ) ;
#531 = CARTESIAN_POINT ( 'NONE',  ( -3.756430356249997882, 25.40312499938548285, 11.16877607737301226 ) ) ;
#532 = EDGE_CURVE ( 'NONE', #18639, #8603, #9423, .T. ) ;
#533 = DIRECTION ( 'NONE',  ( 1.000000000000000000, 0.000000000000000000, 0.000000000000000000 ) ) ;
#534 = CARTESIAN_POINT ( 'NONE',  ( -6.317933499822993682, 30.45149776762736593, -6.500000000000000000 ) ) ;
#535 = CARTESIAN_POINT ( 'NONE',  ( -1.878215178124998497, 26.34062499938548285, 12.25316411605951927 ) ) ;
#536 = DIRECTION ( 'NONE',  ( -0.000000000000000000, -0.000000000000000000, -1.000000000000000000 ) ) ;
#537 = CARTESIAN_POINT ( 'NONE',  ( 0.000000000000000000, 0.000000000000000000, 19.50000000000000000 ) ) ;
#538 = DIRECTION ( 'NONE',  ( 0.000000000000000000, 0.000000000000000000, 1.000000000000000000 ) ) ;
#539 = EDGE_CURVE ( 'NONE', #19632, #14821, #9847, .T. ) ;
#540 = CARTESIAN_POINT ( 'NONE',  ( 1.999999999999998224, -29.29374999877096997, 12.46410161513774639 ) ) ;
#541 = CARTESIAN_POINT ( 'NONE',  ( -25.75859848311247902, 16.66421332384710752, -6.500000000000000000 ) ) ;
#542 = CARTESIAN_POINT ( 'NONE',  ( 21.21320343559646915, 21.21320343559638744, 12.99999999999999289 ) ) ;
#543 = DIRECTION ( 'NONE',  ( 0.000000000000000000, 0.000000000000000000, 1.000000000000000000 ) ) ;
#544 = CARTESIAN_POINT ( 'NONE',  ( 1.290629128713961293, -29.97320584640673147, 5.204870533884474071 ) ) ;
#545 = EDGE_LOOP ( 'NONE', ( #9181, #12765, #6775, #14139, #18806, #21870, #16789, #2419 ) ) ;
#546 = EDGE_CURVE ( 'NONE', #10805, #16184, #12212, .T. ) ;
#547 = CARTESIAN_POINT ( 'NONE',  ( -3.401318489840662540, 30.91344420362552015, -2.750000000000000000 ) ) ;
#549 = ORIENTED_EDGE ( 'NONE', *, *, #7631, .F. ) ;
#548 = LINE ( 'NONE', #4449, #1635 ) ;
#550 = ORIENTED_EDGE ( 'NONE', *, *, #1133, .T. ) ;
#551 = ORIENTED_EDGE ( 'NONE', *, *, #25079, .T. ) ;
#552 = ORIENTED_EDGE ( 'NONE', *, *, #7442, .T. ) ;
#553 = ORIENTED_EDGE ( 'NONE', *, *, #15758, .T. ) ;
#554 = ORIENTED_EDGE ( 'NONE', *, *, #16174, .F. ) ;
#555 = CARTESIAN_POINT ( 'NONE',  ( -4.000000000000003553, -27.73750000000000071, 6.690598923241489970 ) ) ;
#556 = AXIS2_PLACEMENT_3D ( 'NONE', #19, #15717, #3807 ) ;
#557 = EDGE_LOOP ( 'NONE', ( #23842, #6060, #17814, #23687, #3257, #25679 ) ) ;
#558 = DIRECTION ( 'NONE',  ( 0.000000000000000000, 1.000000000000000000, 0.000000000000000000 ) ) ;
#559 = CARTESIAN_POINT ( 'NONE',  ( 3.756430356250002323, 26.56562499938548783, 11.16877607737301403 ) ) ;
#560 = CIRCLE ( 'NONE', #21439, 0.5000000000000005551 ) ;
#561 = CARTESIAN_POINT ( 'NONE',  ( -1.878215178124998497, -12.25316411605951927, 2.353124999385485694 ) ) ;
#562 = CARTESIAN_POINT ( 'NONE',  ( -8.217531866530787710, 29.99470236596041772, -2.750000000000000000 ) ) ;
#563 = CARTESIAN_POINT ( 'NONE',  ( 21.73261250872320716, 16.42021775280438689, 6.831223922626973533 ) ) ;
#564 = CARTESIAN_POINT ( 'NONE',  ( -28.91604871112448549, 11.44867358849382910, -6.500000000000000000 ) ) ;
#565 = AXIS2_PLACEMENT_3D ( 'NONE', #15634, #17845, #20049 ) ;
#566 = DIRECTION ( 'NONE',  ( 0.000000000000000000, 0.000000000000000000, 1.000000000000000000 ) ) ;
#567 = CONTEXT_DEPENDENT_SHAPE_REPRESENTATION ( #13615, #20948 ) ;
#568 = CARTESIAN_POINT ( 'NONE',  ( 3.756430356250004099, -6.831223922626973533, 2.428124999385481431 ) ) ;
#569 =( LENGTH_UNIT ( ) NAMED_UNIT ( * ) SI_UNIT ( .MILLI., .METRE. ) );
#570 = CARTESIAN_POINT ( 'NONE',  ( -1.071796769724487230, 27.77634618820330559, 4.999999999999992006 ) ) ;
#571 = DIRECTION ( 'NONE',  ( 1.000000000000000000, 0.000000000000000000, 0.000000000000000000 ) ) ;
#572 = CARTESIAN_POINT ( 'NONE',  ( -1.878215178124998497, 29.04062499938548569, 12.25316411605951927 ) ) ;
#573 = CARTESIAN_POINT ( 'NONE',  ( -1.878215178124998497, -12.25316411605951927, 1.453124999385484228 ) ) ;
#574 = FACE_OUTER_BOUND ( 'NONE', #3616, .T. ) ;
#575 = ORIENTED_EDGE ( 'NONE', *, *, #4755, .F. ) ;
#576 = EDGE_CURVE ( 'NONE', #5530, #3462, #15285, .T. ) ;
#577 = EDGE_LOOP ( 'NONE', ( #12034, #4407, #15009, #19434 ) ) ;
#578 = CARTESIAN_POINT ( 'NONE',  ( -1.878215178124999829, 26.90312499938548640, 12.25316411605951927 ) ) ;
#579 = EDGE_CURVE ( 'NONE', #21691, #25452, #21965, .T. ) ;
#580 = ORIENTED_EDGE ( 'NONE', *, *, #2262, .F. ) ;
#581 = CARTESIAN_POINT ( 'NONE',  ( 1.071796769724494336, 25.09240381056766367, 4.999999999999992895 ) ) ;
#582 =( GEOMETRIC_REPRESENTATION_CONTEXT ( 3 ) GLOBAL_UNCERTAINTY_ASSIGNED_CONTEXT ( ( #20915 ) ) GLOBAL_UNIT_ASSIGNED_CONTEXT ( ( #19068, #4949, #20517 ) ) REPRESENTATION_CONTEXT ( 'NONE', 'WORKASPACE' ) );
#583 = VERTEX_POINT ( 'NONE', #20304 ) ;
#584 = CARTESIAN_POINT ( 'NONE',  ( 1.057460391440397258E-14, -28.71250000000000213, 4.999999999999992006 ) ) ;
#585 = VERTEX_POINT ( 'NONE', #10235 ) ;
#586 = CARTESIAN_POINT ( 'NONE',  ( 3.756430356250003655, -8.999999999999992895, 4.640624999385483562 ) ) ;
#587=STYLED_ITEM('',(#25907),#5394);
#588 = CARTESIAN_POINT ( 'NONE',  ( 22.67092431280578779, -21.28941499438234786, -6.500000000000000000 ) ) ;
#589 = ORIENTED_EDGE ( 'NONE', *, *, #21385, .T. ) ;
#590 = FACE_OUTER_BOUND ( 'NONE', #13824, .T. ) ;
#591 = CARTESIAN_POINT ( 'NONE',  ( -1.878215178124995832, 27.54062499938548214, 5.746835883940462963 ) ) ;
#592 = CARTESIAN_POINT ( 'NONE',  ( 1.071796769724487675, 29.14240381056766438, 4.999999999999988454 ) ) ;
#593 = DIRECTION ( 'NONE',  ( -0.000000000000000000, 0.000000000000000000, 1.000000000000000000 ) ) ;
#594 = CARTESIAN_POINT ( 'NONE',  ( 20.53936981547090568, 15.22697505955208896, 6.831223922626973533 ) ) ;
#595 =( GEOMETRIC_REPRESENTATION_CONTEXT ( 3 ) GLOBAL_UNCERTAINTY_ASSIGNED_CONTEXT ( ( #8894 ) ) GLOBAL_UNIT_ASSIGNED_CONTEXT ( ( #1543, #19329, #25603 ) ) REPRESENTATION_CONTEXT ( 'NONE', 'WORKASPACE' ) );
#596 = CARTESIAN_POINT ( 'NONE',  ( -1.878215178124995832, 28.44062499938548427, 5.746835883940462963 ) ) ;
#597 = CARTESIAN_POINT ( 'NONE',  ( 3.369928719974892281E-15, 25.11250000000000426, 4.999999999999992006 ) ) ;
#598 = ADVANCED_FACE ( 'NONE', ( #6456 ), #4362, .F. ) ;
#599 = APPLICATION_CONTEXT ( 'automotive_design' ) ;
#600 = CARTESIAN_POINT ( 'NONE',  ( -0.4995657836784015426, 38.49999999999999289, 3.020833333333323267 ) ) ;
#601 = CARTESIAN_POINT ( 'NONE',  ( 4.000000000000002665, 25.80624999877096926, 11.30940107675849760 ) ) ;
#602 = CARTESIAN_POINT ( 'NONE',  ( 1.859271017917182139E-15, 29.33124999877096428, 12.99999999999999289 ) ) ;
#604 = EDGE_CURVE ( 'NONE', #23841, #1729, #1999, .T. ) ;
#603 = CARTESIAN_POINT ( 'NONE',  ( -2.672651547586948120E-15, -27.72812499938548569, 13.33755215474603162 ) ) ;
#605 = CARTESIAN_POINT ( 'NONE',  ( 5.563387625853419394, 38.77026726007181878, 10.37110993082982979 ) ) ;
#606 = ORIENTED_EDGE ( 'NONE', *, *, #13099, .F. ) ;
#607 = CARTESIAN_POINT ( 'NONE',  ( 3.735045420075836212E-15, 26.26562499938548356, 4.662447845253954171 ) ) ;
#608 = CARTESIAN_POINT ( 'NONE',  ( -3.752267015613588906E-15, -29.16250000000000142, 4.381197846482986158 ) ) ;
#610 = ORIENTED_EDGE ( 'NONE', *, *, #15078, .F. ) ;
#609 = CARTESIAN_POINT ( 'NONE',  ( 3.756430356250002323, 27.46562499938548640, 11.16877607737301403 ) ) ;
#611 = ORIENTED_EDGE ( 'NONE', *, *, #24958, .T. ) ;
#612 = DIRECTION ( 'NONE',  ( 0.000000000000000000, 0.000000000000000000, 1.000000000000000000 ) ) ;
#613 =( BOUNDED_CURVE ( )  B_SPLINE_CURVE ( 2, ( #5584, #19696, #5450, #11464, #9881 ),
 .UNSPECIFIED., .F., .F. ) 
 B_SPLINE_CURVE_WITH_KNOTS ( ( 3, 2, 3 ),
 ( 0.9749999999999999778, 0.9833333333333332815, 1.000000000000000000 ),
 .UNSPECIFIED. ) 
 CURVE ( )  GEOMETRIC_REPRESENTATION_ITEM ( )  RATIONAL_B_SPLINE_CURVE ( ( 0.9330127018922194093, 0.9330127018922194093, 1.000000000000000000, 0.8660254037844387076, 1.000000000000000000 ) ) 
 REPRESENTATION_ITEM ( '' )  );
#614 = CARTESIAN_POINT ( 'NONE',  ( 3.526711513754818395, 29.50000000000000000, 4.145898033750289535 ) ) ;
#615 = ORIENTED_EDGE ( 'NONE', *, *, #13996, .T. ) ;
#616 = ORIENTED_EDGE ( 'NONE', *, *, #17721, .F. ) ;
#617 = CARTESIAN_POINT ( 'NONE',  ( -2.672651547586948120E-15, -26.04062499938548925, 13.33755215474603162 ) ) ;
#618 = CARTESIAN_POINT ( 'NONE',  ( 3.756430356250004987, 27.84062499938548640, 8.999999999999992895 ) ) ;
#619 = CARTESIAN_POINT ( 'NONE',  ( 20.05209915500855544, 18.53634962715644363, 4.999999999999989342 ) ) ;
#620 = EDGE_CURVE ( 'NONE', #5209, #6382, #2280, .T. ) ;
#621 = CARTESIAN_POINT ( 'NONE',  ( 1.500000000000001776, -10.49999999999999289, 25.00000000000000000 ) ) ;
#622 = CARTESIAN_POINT ( 'NONE',  ( 3.469446951953614189E-15, 30.00000000000000355, 4.999999999999992006 ) ) ;
#623 = CARTESIAN_POINT ( 'NONE',  ( 18.60454468811453310, 20.12029421596650991, 4.999999999999992006 ) ) ;
#624 = FACE_OUTER_BOUND ( 'NONE', #15797, .T. ) ;
#625 = DIRECTION ( 'NONE',  ( 1.000000000000000000, 0.000000000000000000, 0.000000000000000000 ) ) ;
#626 = CARTESIAN_POINT ( 'NONE',  ( 16.89751483010538990, 22.20990958602406451, 11.16877607737301226 ) ) ;
#627 = CARTESIAN_POINT ( 'NONE',  ( 18.87533163942939041, 21.70375876417550032, 5.535898384862237620 ) ) ;
#628 = CARTESIAN_POINT ( 'NONE',  ( 23.96650046397252609, 18.30964621448006824, 8.999999999999992895 ) ) ;
#629 = CARTESIAN_POINT ( 'NONE',  ( 23.66156066545488201, 18.00470641596242771, 11.30940107675849760 ) ) ;
#630 = CARTESIAN_POINT ( 'NONE',  ( 1.878215178125004048, 26.56562499938548427, 5.746835883940462963 ) ) ;
#632 = EDGE_LOOP ( 'NONE', ( #6319, #11612, #8419, #5612 ) ) ;
#631 = FACE_OUTER_BOUND ( 'NONE', #5269, .T. ) ;
#633 = CARTESIAN_POINT ( 'NONE',  ( -3.999999999999998224, 25.61874999877097281, 8.999999999999992895 ) ) ;
#634 = CARTESIAN_POINT ( 'NONE',  ( -18.68225429291695860, 24.86329371854795056, -2.750000000000000000 ) ) ;
#635 = ORIENTED_EDGE ( 'NONE', *, *, #10538, .T. ) ;
#636 = PLANE ( 'NONE',  #20950 ) ;
#637 = CARTESIAN_POINT ( 'NONE',  ( 2.000000000000000888, 27.56874999877096855, 12.46410161513774817 ) ) ;
#638 = CARTESIAN_POINT ( 'NONE',  ( 3.756430356249995661, -25.77812499938548640, 6.831223922626973533 ) ) ;
#640 = ORIENTED_EDGE ( 'NONE', *, *, #22909, .T. ) ;
#639 = DIRECTION ( 'NONE',  ( 0.000000000000000000, 1.000000000000000000, -0.000000000000000000 ) ) ;
#641 = CYLINDRICAL_SURFACE ( 'NONE', #13338, 0.5000000000000004441 ) ;
#642 = EDGE_CURVE ( 'NONE', #8421, #20150, #12769, .T. ) ;
#643 = ORIENTED_EDGE ( 'NONE', *, *, #9008, .T. ) ;
#644 = CARTESIAN_POINT ( 'NONE',  ( 3.756430356249995661, -25.32812499938548356, 6.831223922626973533 ) ) ;
#645 = ORIENTED_EDGE ( 'NONE', *, *, #15056, .T. ) ;
#646 = ORIENTED_EDGE ( 'NONE', *, *, #19907, .T. ) ;
#647 = DIRECTION ( 'NONE',  ( -0.000000000000000000, 0.000000000000000000, -1.000000000000000000 ) ) ;
#648 = DIRECTION ( 'NONE',  ( -0.000000000000000000, -0.000000000000000000, 1.000000000000000000 ) ) ;
#649 = EDGE_CURVE ( 'NONE', #12662, #14524, #9982, .T. ) ;
#650 = CIRCLE ( 'NONE', #19423, 31.10000000000000142 ) ;
#651 = CARTESIAN_POINT ( 'NONE',  ( 4.000000000000032863, -11.30940107675847983, 3.506249998770968102 ) ) ;
#652 = CARTESIAN_POINT ( 'NONE',  ( 1.878215178125004048, -5.746835883940462963, 1.228124999385484584 ) ) ;
#653 = CARTESIAN_POINT ( 'NONE',  ( -3.369928719974892281E-15, -25.50624999877096855, 4.999999999999992006 ) ) ;
#654 = CARTESIAN_POINT ( 'NONE',  ( 3.756430356250002323, 26.00312499938548427, 11.16877607737301226 ) ) ;
#655 = LINE ( 'NONE', #10968, #1709 ) ;
#656 = DIRECTION ( 'NONE',  ( 0.000000000000000000, -1.000000000000000000, -0.000000000000000000 ) ) ;
#657 = CARTESIAN_POINT ( 'NONE',  ( 3.756430356250003211, 28.32812499938548356, 6.831223922626973533 ) ) ;
#658 = DIRECTION ( 'NONE',  ( 0.000000000000000000, 0.000000000000000000, -1.000000000000000000 ) ) ;
#659 = CARTESIAN_POINT ( 'NONE',  ( -28.91604871112473418, -11.44867358849319849, -6.500000000000000000 ) ) ;
#660 = CARTESIAN_POINT ( 'NONE',  ( -3.999999999999997335, 28.80624999877096926, 11.30940107675849404 ) ) ;
#661 = CARTESIAN_POINT ( 'NONE',  ( -3.735045420075836212E-15, -27.16562499938548569, 4.662447845253954171 ) ) ;
#662 = DIRECTION ( 'NONE',  ( -0.000000000000000000, -0.000000000000000000, 1.000000000000000000 ) ) ;
#663 = CARTESIAN_POINT ( 'NONE',  ( 3.999999999999996447, -26.12500000000000355, 8.999999999999992895 ) ) ;
#664 = CARTESIAN_POINT ( 'NONE',  ( 1.999999999999995781, -25.15000000000000213, 5.535898384862237620 ) ) ;
#665 = CARTESIAN_POINT ( 'NONE',  ( 3.974007292349814424, -29.73566758725665338, 9.525109153848150711 ) ) ;
#666 = ORIENTED_EDGE ( 'NONE', *, *, #17227, .T. ) ;
#667 = DIRECTION ( 'NONE',  ( 0.000000000000000000, -1.000000000000000000, 0.000000000000000000 ) ) ;
#669 = ORIENTED_EDGE ( 'NONE', *, *, #3778, .F. ) ;
#668 = CARTESIAN_POINT ( 'NONE',  ( -3.999999999999995559, -6.690598923241487306, 3.731249998770965970 ) ) ;
#671 = EDGE_LOOP ( 'NONE', ( #19623, #22738 ) ) ;
#670 = EDGE_CURVE ( 'NONE', #18554, #13915, #7548, .T. ) ;
#672 = VERTEX_POINT ( 'NONE', #12072 ) ;
#673 = ORIENTED_EDGE ( 'NONE', *, *, #14998, .F. ) ;
#674 = VERTEX_POINT ( 'NONE', #20047 ) ;
#675 = CARTESIAN_POINT ( 'NONE',  ( 0.000000000000000000, 0.000000000000000000, -6.500000000000000000 ) ) ;
#676 = ADVANCED_FACE ( 'NONE', ( #6327 ), #18231, .F. ) ;
#677 = ORIENTED_EDGE ( 'NONE', *, *, #7902, .T. ) ;
#678 = AXIS2_PLACEMENT_3D ( 'NONE', #25811, #10355, #2014 ) ;
#679 = ADVANCED_FACE ( 'NONE', ( #8163 ), #16144, .T. ) ;
#680 = CARTESIAN_POINT ( 'NONE',  ( 0.000000000000000000, 0.000000000000000000, -6.500000000000000000 ) ) ;
#681 = CARTESIAN_POINT ( 'NONE',  ( 1.878215178125000939, 28.77812499938548640, 12.25316411605952283 ) ) ;
#682 = CARTESIAN_POINT ( 'NONE',  ( 3.756430356250004099, -6.831223922626973533, 3.440624999385483829 ) ) ;
#683 = DIRECTION ( 'NONE',  ( -0.000000000000000000, -1.000000000000000000, -0.000000000000000000 ) ) ;
#684 = CARTESIAN_POINT ( 'NONE',  ( 17.53391093317328142, 22.84630568909195958, 11.16877607737301226 ) ) ;
#685 = ADVANCED_FACE ( 'NONE', ( #14177 ), #22147, .F. ) ;
#686 = DIRECTION ( 'NONE',  ( -0.000000000000000000, -0.000000000000000000, -1.000000000000000000 ) ) ;
#687 = CARTESIAN_POINT ( 'NONE',  ( -3.999999999999953371, -6.690598923241463325, 0.6374999999999958478 ) ) ;
#688 = ITEM_DEFINED_TRANSFORMATION ( 'NONE', 'NONE', #11032,  #21036 ) ;
#689 = CARTESIAN_POINT ( 'NONE',  ( -1.878215178124998497, -12.25316411605951927, 0.8906249993854836733 ) ) ;
#690 = FACE_OUTER_BOUND ( 'NONE', #16797, .T. ) ;
#691 = CARTESIAN_POINT ( 'NONE',  ( -18.28012134629613783, -25.16042852506070560, -6.500000000000000000 ) ) ;
#692 = CYLINDRICAL_SURFACE ( 'NONE', #17204, 0.5000000000000002220 ) ;
#693 = DIRECTION ( 'NONE',  ( 0.000000000000000000, 0.000000000000000000, 1.000000000000000000 ) ) ;
#694 = CARTESIAN_POINT ( 'NONE',  ( -1.878215178124995832, -5.746835883940462963, 2.653124999385483740 ) ) ;
#695 = CARTESIAN_POINT ( 'NONE',  ( -1.626862140677534194E-14, -28.03750000000000497, 12.99999999999999289 ) ) ;
#696 = AXIS2_PLACEMENT_3D ( 'NONE', #9375, #6205, #16157 ) ;
#697 = ORIENTED_EDGE ( 'NONE', *, *, #18302, .T. ) ;
#698 = ORIENTED_EDGE ( 'NONE', *, *, #8966, .F. ) ;
#699 = CARTESIAN_POINT ( 'NONE',  ( 3.756430356250004543, 28.81562499938548783, 11.16877607737301226 ) ) ;
#700 = EDGE_LOOP ( 'NONE', ( #21687, #12958, #18424, #6447 ) ) ;
#701 = DIRECTION ( 'NONE',  ( 0.06279051952932236669, 0.9980267284282710039, 0.000000000000000000 ) ) ;
#702 = VERTEX_POINT ( 'NONE', #9421 ) ;
#703 = ORIENTED_EDGE ( 'NONE', *, *, #17786, .T. ) ;
#704 = CARTESIAN_POINT ( 'NONE',  ( -1.071796769724485232, 27.77634618820331269, 4.999999999999992006 ) ) ;
#705 = ORIENTED_EDGE ( 'NONE', *, *, #13948, .T. ) ;
#706 = CARTESIAN_POINT ( 'NONE',  ( 1.071796769724494558, 28.63615380933863364, 4.999999999999992895 ) ) ;
#707 = EDGE_CURVE ( 'NONE', #19701, #5616, #22374, .T. ) ;
#708 = CARTESIAN_POINT ( 'NONE',  ( -3.756430356249996994, 28.51562499938548356, 8.999999999999992895 ) ) ;
#709 = CARTESIAN_POINT ( 'NONE',  ( 16.28113363682029657, 21.93798788631260877, 8.999999999999992895 ) ) ;
#710 = CARTESIAN_POINT ( 'NONE',  ( 4.000000000000001776, 26.76250000000000284, 11.30940107675849760 ) ) ;
#711 = LINE ( 'NONE', #8815, #3315 ) ;
#712 = CARTESIAN_POINT ( 'NONE',  ( 19.23778763078571430, 16.58159025282627397, 5.746835883940462963 ) ) ;
#713 = ADVANCED_FACE ( 'NONE', ( #25117 ), #1318, .F. ) ;
#714 = EDGE_CURVE ( 'NONE', #10206, #12794, #12708, .T. ) ;
#715 = CARTESIAN_POINT ( 'NONE',  ( 3.735045420075836212E-15, 28.40312499938548640, 4.662447845253954171 ) ) ;
#716 = CARTESIAN_POINT ( 'NONE',  ( 19.55598568231966539, 16.89978830436022150, 5.746835883940462963 ) ) ;
#717 = CARTESIAN_POINT ( 'NONE',  ( 20.14370442905180880, 20.14370442905173775, 13.61880215351699874 ) ) ;
#718 = CARTESIAN_POINT ( 'NONE',  ( 0.000000000000000000, 25.73124999877097352, 13.61880215351699874 ) ) ;
#719 = CARTESIAN_POINT ( 'NONE',  ( 3.959305671612554781E-15, 35.50000000000000711, 12.99999999999999289 ) ) ;
#720 = CARTESIAN_POINT ( 'NONE',  ( -3.735045420075836212E-15, -27.05312499938548498, 4.662447845253954171 ) ) ;
#721 = CARTESIAN_POINT ( 'NONE',  ( -1.057460391440397258E-14, 28.71250000000000213, 4.999999999999992006 ) ) ;
#722 = EDGE_LOOP ( 'NONE', ( #1470, #16759, #21538, #23056 ) ) ;
#723 = CARTESIAN_POINT ( 'NONE',  ( 3.756430356250003655, 26.15312499938548640, 8.999999999999992895 ) ) ;
#724 = CARTESIAN_POINT ( 'NONE',  ( 1.999999999999995781, -28.75000000000000000, 5.535898384862237620 ) ) ;
#726 = ORIENTED_EDGE ( 'NONE', *, *, #19375, .T. ) ;
#725 = DIRECTION ( 'NONE',  ( -0.000000000000000000, -0.000000000000000000, -1.000000000000000000 ) ) ;
#727 = ORIENTED_EDGE ( 'NONE', *, *, #13164, .F. ) ;
#728 = CARTESIAN_POINT ( 'NONE',  ( 3.756430356250003655, 29.75312499938548783, 8.999999999999992895 ) ) ;
#729 = DIRECTION ( 'NONE',  ( 0.000000000000000000, 0.000000000000000000, -1.000000000000000000 ) ) ;
#730 = ORIENTED_EDGE ( 'NONE', *, *, #5993, .T. ) ;
#731 = CARTESIAN_POINT ( 'NONE',  ( 1.878215178124995832, -26.75312499938548783, 5.746835883940462963 ) ) ;
#732 = LINE ( 'NONE', #6998, #10114 ) ;
#733 = DIRECTION ( 'NONE',  ( 0.000000000000000000, 0.000000000000000000, 1.000000000000000000 ) ) ;
#734 = LINE ( 'NONE', #6878, #984 ) ;
#735 = CARTESIAN_POINT ( 'NONE',  ( 3.756430356250003211, 26.04062499938548925, 8.999999999999992895 ) ) ;
#736 = ADVANCED_FACE ( 'NONE', ( #18500 ), #8555, .F. ) ;
#737 = CARTESIAN_POINT ( 'NONE',  ( -3.999999999999996447, -8.999999999999992895, 1.125000000000000888 ) ) ;
#738 = FILL_AREA_STYLE_COLOUR ( '', #17309 ) ;
#739 =( BOUNDED_CURVE ( )  B_SPLINE_CURVE ( 2, ( #20311, #10242, #24247, #15891, #16419, #18125, #8045, #19919, #14185 ),
 .UNSPECIFIED., .F., .F. ) 
 B_SPLINE_CURVE_WITH_KNOTS ( ( 3, 2, 2, 2, 3 ),
 ( 0.8750000000000000000, 0.8833333333333333037, 0.9000000000000000222, 0.9166666666666666297, 0.9250000000000000444 ),
 .UNSPECIFIED. ) 
 CURVE ( )  GEOMETRIC_REPRESENTATION_ITEM ( )  RATIONAL_B_SPLINE_CURVE ( ( 0.9330127018922194093, 0.9330127018922194093, 1.000000000000000000, 0.8660254037844387076, 1.000000000000000000, 0.8660254037844387076, 1.000000000000000000, 0.9330127018922189652, 0.9330127018922194093 ) ) 
 REPRESENTATION_ITEM ( '' )  );
#740 = CARTESIAN_POINT ( 'NONE',  ( -28.91604871112473418, -11.44867358849319849, -6.500000000000000000 ) ) ;
#741 = EDGE_CURVE ( 'NONE', #14667, #12275, #23629, .T. ) ;
#742 = CARTESIAN_POINT ( 'NONE',  ( -30.54913349766215802, 5.827558883616378083, -6.500000000000000000 ) ) ;
#743 = FACE_OUTER_BOUND ( 'NONE', #23538, .T. ) ;
#744 = CARTESIAN_POINT ( 'NONE',  ( 1.999999999999995781, -28.24374999877096570, 5.535898384862237620 ) ) ;
#745 = CARTESIAN_POINT ( 'NONE',  ( 16.23460222274299980, 21.54699697866167440, 8.999999999999992895 ) ) ;
#746 = CARTESIAN_POINT ( 'NONE',  ( 20.19238178538755690, 17.53618440742811302, 5.746835883940462963 ) ) ;
#747 = FACE_OUTER_BOUND ( 'NONE', #11528, .T. ) ;
#748 =( BOUNDED_CURVE ( )  B_SPLINE_CURVE ( 2, ( #10541, #623, #16571, #872, #4915, #24529, #14867, #6614, #12897 ),
 .UNSPECIFIED., .F., .F. ) 
 B_SPLINE_CURVE_WITH_KNOTS ( ( 3, 2, 2, 2, 3 ),
 ( 0.5250000000000000222, 0.5333333333333333259, 0.5500000000000000444, 0.5666666666666666519, 0.5750000000000000666 ),
 .UNSPECIFIED. ) 
 CURVE ( )  GEOMETRIC_REPRESENTATION_ITEM ( )  RATIONAL_B_SPLINE_CURVE ( ( 0.9330127018922194093, 0.9330127018922194093, 1.000000000000000000, 0.8660254037844387076, 1.000000000000000000, 0.8660254037844387076, 1.000000000000000000, 0.9330127018922189652, 0.9330127018922194093 ) ) 
 REPRESENTATION_ITEM ( '' )  );
#749 = CARTESIAN_POINT ( 'NONE',  ( 3.735045420075836212E-15, 25.25312499938548783, 4.662447845253954171 ) ) ;
#751 = ORIENTED_EDGE ( 'NONE', *, *, #3136, .F. ) ;
#750 = DIRECTION ( 'NONE',  ( 0.000000000000000000, 0.000000000000000000, -1.000000000000000000 ) ) ;
#752 = CARTESIAN_POINT ( 'NONE',  ( 19.68856820379214057, 17.03237082583270023, 12.25316411605952283 ) ) ;
#753 = ORIENTED_EDGE ( 'NONE', *, *, #6718, .T. ) ;
#754 = DIRECTION ( 'NONE',  ( 0.9921147013144777649, -0.1253332335643050077, 0.000000000000000000 ) ) ;
#755 = CARTESIAN_POINT ( 'NONE',  ( 4.000000000000001776, 27.60624999877096641, 11.30940107675849760 ) ) ;
#756 = CARTESIAN_POINT ( 'NONE',  ( -2.672651547586948120E-15, -27.72812499938548569, 13.33755215474602984 ) ) ;
#758 = EDGE_LOOP ( 'NONE', ( #1820, #6628, #21819, #13928 ) ) ;
#757 = CARTESIAN_POINT ( 'NONE',  ( -23.96296185032722548, -19.82388608118403539, -6.500000000000000000 ) ) ;
#759 = CARTESIAN_POINT ( 'NONE',  ( 4.000000000000001776, 29.89374999877097139, 8.999999999999992895 ) ) ;
#760 = ORIENTED_EDGE ( 'NONE', *, *, #22579, .T. ) ;
#761 = CARTESIAN_POINT ( 'NONE',  ( -3.756430356250004099, -29.34062499938548640, 6.831223922626973533 ) ) ;
#762 = EDGE_LOOP ( 'NONE', ( #22709, #20677, #24398, #5708 ) ) ;
#763 = ORIENTED_EDGE ( 'NONE', *, *, #18899, .F. ) ;
#764 = FILL_AREA_STYLE_COLOUR ( '', #25582 ) ;
#765 = CARTESIAN_POINT ( 'NONE',  ( -3.756430356249996105, 25.44062499938548783, 6.831223922626973533 ) ) ;
#766 = AXIS2_PLACEMENT_3D ( 'NONE', #19619, #9699, #1586 ) ;
#767 = CARTESIAN_POINT ( 'NONE',  ( 1.071796769724494558, 27.79240381056766651, 4.999999999999992895 ) ) ;
#768 = ADVANCED_FACE ( 'NONE', ( #3150 ), #24982, .T. ) ;
#769 = EDGE_CURVE ( 'NONE', #20241, #8698, #8602, .T. ) ;
#770 = CARTESIAN_POINT ( 'NONE',  ( -3.756430356249995661, -6.831223922626973533, 0.8906249993854814528 ) ) ;
#771 = LINE ( 'NONE', #23004, #7188 ) ;
#772 = CARTESIAN_POINT ( 'NONE',  ( 3.756430356250002323, 27.80312499938548143, 11.16877607737301226 ) ) ;
#773 = DIRECTION ( 'NONE',  ( 0.000000000000000000, 0.000000000000000000, 1.000000000000000000 ) ) ;
#774 = UNCERTAINTY_MEASURE_WITH_UNIT (LENGTH_MEASURE( 1.000000000000000082E-05 ), #11385, 'distance_accuracy_value', 'NONE');
#775 = CARTESIAN_POINT ( 'NONE',  ( -3.756430356249996994, 29.41562499938548569, 8.999999999999992895 ) ) ;
#776 = CARTESIAN_POINT ( 'NONE',  ( 3.469446951953614189E-15, -8.999999999999992895, 18.00000000000000000 ) ) ;
#777 = CARTESIAN_POINT ( 'NONE',  ( 23.01498157845693981, 19.24484030382106781, 11.99618178085344589 ) ) ;
#778 = CARTESIAN_POINT ( 'NONE',  ( 1.859271017917182139E-15, 28.88124999877096499, 12.99999999999999289 ) ) ;
#779 = CARTESIAN_POINT ( 'NONE',  ( 3.756430356249996994, -27.72812499938548569, 8.999999999999992895 ) ) ;
#780 = CARTESIAN_POINT ( 'NONE',  ( -3.756430356249997882, 29.56562499938549138, 11.16877607737301226 ) ) ;
#782 = EDGE_CURVE ( 'NONE', #17013, #7673, #14861, .T. ) ;
#781 = DIRECTION ( 'NONE',  ( -0.8763066800438602533, 0.4817536741017213187, 0.000000000000000000 ) ) ;
#783 = AXIS2_PLACEMENT_3D ( 'NONE', #21558, #5346, #13473 ) ;
#784 = CARTESIAN_POINT ( 'NONE',  ( 1.071796769724487230, -25.13259618943233420, 4.999999999999992006 ) ) ;
#785 = PLANE ( 'NONE',  #21415 ) ;
#786 = ORIENTED_EDGE ( 'NONE', *, *, #24587, .F. ) ;
#787 = DIRECTION ( 'NONE',  ( 0.000000000000000000, 0.000000000000000000, 1.000000000000000000 ) ) ;
#789 = VERTEX_POINT ( 'NONE', #1451 ) ;
#788 = DIRECTION ( 'NONE',  ( -0.000000000000000000, -0.000000000000000000, 1.000000000000000000 ) ) ;
#790 = VECTOR ( 'NONE', #20010, 1000.000000000000000 ) ;
#791 = ORIENTED_EDGE ( 'NONE', *, *, #22163, .F. ) ;
#793 = ORIENTED_EDGE ( 'NONE', *, *, #4739, .F. ) ;
#792 = AXIS2_PLACEMENT_3D ( 'NONE', #15459, #16816, #19491 ) ;
#794 = ORIENTED_EDGE ( 'NONE', *, *, #11379, .T. ) ;
#795 = ORIENTED_EDGE ( 'NONE', *, *, #23095, .F. ) ;
#796 = CARTESIAN_POINT ( 'NONE',  ( 27.09999999999999787, -0.5999999999999998668, 19.00000000000000000 ) ) ;
#797 = ORIENTED_EDGE ( 'NONE', *, *, #18776, .F. ) ;
#798 = DIRECTION ( 'NONE',  ( -0.000000000000000000, -0.000000000000000000, -1.000000000000000000 ) ) ;
#799 = CARTESIAN_POINT ( 'NONE',  ( -1.878215178124998497, 29.15312499938548640, 12.25316411605951927 ) ) ;
#800 = AXIS2_PLACEMENT_3D ( 'NONE', #15650, #15525, #5578 ) ;
#801 = CARTESIAN_POINT ( 'NONE',  ( 2.672651547586948120E-15, -13.33755215474602984, 4.640624999385483562 ) ) ;
#802 = AXIS2_PLACEMENT_3D ( 'NONE', #2935, #3450, #11424 ) ;
#803 = CARTESIAN_POINT ( 'NONE',  ( 1.859271017917182139E-15, 28.48749999999999716, 12.99999999999999289 ) ) ;
#804 = LINE ( 'NONE', #24741, #11411 ) ;
#805 = CARTESIAN_POINT ( 'NONE',  ( 3.756430356250003655, 25.70312499938548356, 8.999999999999992895 ) ) ;
#806 = AXIS2_PLACEMENT_3D ( 'NONE', #20605, #12487, #857 ) ;
#807 = AXIS2_PLACEMENT_3D ( 'NONE', #14101, #23650, #10169 ) ;
#809 = EDGE_CURVE ( 'NONE', #24918, #4288, #17286, .T. ) ;
#808 = CARTESIAN_POINT ( 'NONE',  ( -1.878215178124995832, -5.746835883940462963, 3.890624999385482674 ) ) ;
#810 = DIRECTION ( 'NONE',  ( -0.000000000000000000, -1.000000000000000000, 0.000000000000000000 ) ) ;
#811 = CARTESIAN_POINT ( 'NONE',  ( -1.999999999999995781, -5.535898384862237620, 3.750000000000000000 ) ) ;
#812 = CARTESIAN_POINT ( 'NONE',  ( 0.000000000000000000, 0.000000000000000000, -6.500000000000000000 ) ) ;
#813 = CARTESIAN_POINT ( 'NONE',  ( -3.999999999999996447, 29.63124999877097210, 6.690598923241487306 ) ) ;
#814 = CARTESIAN_POINT ( 'NONE',  ( -3.756430356249996105, -6.831223922626973533, 3.140624999385484006 ) ) ;
#815 = CYLINDRICAL_SURFACE ( 'NONE', #1171, 4.000000000000000000 ) ;
#816 = DIRECTION ( 'NONE',  ( 0.000000000000000000, 0.000000000000000000, 1.000000000000000000 ) ) ;
#817 = ORIENTED_EDGE ( 'NONE', *, *, #17018, .F. ) ;
#818 = ORIENTED_EDGE ( 'NONE', *, *, #7336, .T. ) ;
#819 = CARTESIAN_POINT ( 'NONE',  ( 1.878215178125003382, 28.02812499938548996, 5.746835883940462963 ) ) ;
#820 = AXIS2_PLACEMENT_3D ( 'NONE', #8589, #18784, #24666 ) ;
#822 = VERTEX_POINT ( 'NONE', #12458 ) ;
#821 = AXIS2_PLACEMENT_3D ( 'NONE', #376, #22462, #6254 ) ;
#823 = DIRECTION ( 'NONE',  ( -0.1873813145857119722, 0.9822872507286911636, 0.000000000000000000 ) ) ;
#824 = ORIENTED_EDGE ( 'NONE', *, *, #17375, .F. ) ;
#825 = CARTESIAN_POINT ( 'NONE',  ( 1.878215178124998497, -26.00312499938548783, 12.25316411605951927 ) ) ;
#826 = EDGE_LOOP ( 'NONE', ( #3312, #6963, #2563, #11339 ) ) ;
#827 = CARTESIAN_POINT ( 'NONE',  ( 23.26836714124207361, 18.93629030671969460, 11.57226653943512851 ) ) ;
#828 = AXIS2_PLACEMENT_3D ( 'NONE', #14567, #3180, #16661 ) ;
#829 = VECTOR ( 'NONE', #20995, 1000.000000000000000 ) ;
#830 = ORIENTED_EDGE ( 'NONE', *, *, #3925, .F. ) ;
#831 = FACE_OUTER_BOUND ( 'NONE', #14793, .T. ) ;
#832 = CARTESIAN_POINT ( 'NONE',  ( 1.878215178125000939, 29.11562499938548498, 12.25316411605952283 ) ) ;
#833 = CARTESIAN_POINT ( 'NONE',  ( 3.999999999999995559, -27.43750000000000000, 6.690598923241487306 ) ) ;
#834 = AXIS2_PLACEMENT_3D ( 'NONE', #5383, #9320, #12752 ) ;
#835 = FACE_OUTER_BOUND ( 'NONE', #22363, .T. ) ;
#836 = CARTESIAN_POINT ( 'NONE',  ( 3.834746474454188013E-15, 28.20624999877096428, 4.999999999999992006 ) ) ;
#837 = CARTESIAN_POINT ( 'NONE',  ( 16.97706434298888212, 22.28945909890755317, 11.16877607737301226 ) ) ;
#838 = AXIS2_PLACEMENT_3D ( 'NONE', #8930, #15201, #10864 ) ;
#839 = CARTESIAN_POINT ( 'NONE',  ( 3.756430356250003655, 29.19062499938548072, 8.999999999999992895 ) ) ;
#840 = AXIS2_PLACEMENT_3D ( 'NONE', #2316, #10272, #20617 ) ;
#841 = EDGE_CURVE ( 'NONE', #11726, #2271, #16535, .T. ) ;
#842 = CARTESIAN_POINT ( 'NONE',  ( 16.95282131294928263, 19.60901869090858796, 5.746835883940462963 ) ) ;
#843 = CARTESIAN_POINT ( 'NONE',  ( 20.85081121023834427, 15.19395696074590596, 6.690598923241489970 ) ) ;
#844 = ORIENTED_EDGE ( 'NONE', *, *, #18813, .T. ) ;
#845 = CARTESIAN_POINT ( 'NONE',  ( -1.071796769724494336, -25.09240381056766367, 4.999999999999992895 ) ) ;
#846 = EDGE_CURVE ( 'NONE', #3229, #3397, #21536, .T. ) ;
#847 = CARTESIAN_POINT ( 'NONE',  ( -3.999999999999996447, 26.48124999877096997, 6.690598923241487306 ) ) ;
#848 = CARTESIAN_POINT ( 'NONE',  ( -1.878215178125000939, -26.41562499938548214, 12.25316411605952283 ) ) ;
#849 = CARTESIAN_POINT ( 'NONE',  ( 5.428131658003001903, 38.61087488181073724, 11.28411968614168615 ) ) ;
#850 = AXIS2_PLACEMENT_3D ( 'NONE', #16943, #22823, #13265 ) ;
#851 = CARTESIAN_POINT ( 'NONE',  ( -3.999999999999996003, 29.18124999877096926, 6.690598923241487306 ) ) ;
#852 = CARTESIAN_POINT ( 'NONE',  ( 4.000000000000003553, 29.89374999877096784, 8.999999999999992895 ) ) ;
#853 = EDGE_CURVE ( 'NONE', #12237, #5263, #24888, .T. ) ;
#855 = VERTEX_POINT ( 'NONE', #17017 ) ;
#854 = DIRECTION ( 'NONE',  ( 0.000000000000000000, 0.000000000000000000, 1.000000000000000000 ) ) ;
#856 = ORIENTED_EDGE ( 'NONE', *, *, #17515, .T. ) ;
#857 = DIRECTION ( 'NONE',  ( -1.000000000000000000, 0.000000000000000000, 0.000000000000000000 ) ) ;
#858 = AXIS2_PLACEMENT_3D ( 'NONE', #20378, #18188, #10066 ) ;
#859 = AXIS2_PLACEMENT_3D ( 'NONE', #19011, #19263, #3062 ) ;
#860 = CARTESIAN_POINT ( 'NONE',  ( 3.999999999999956035, -11.30940107675852602, 4.406249998770962684 ) ) ;
#861 = ORIENTED_EDGE ( 'NONE', *, *, #11086, .T. ) ;
#862 = CARTESIAN_POINT ( 'NONE',  ( 1.878215178124995832, -27.20312499938548711, 5.746835883940462963 ) ) ;
#863 = DIRECTION ( 'NONE',  ( 0.000000000000000000, 0.000000000000000000, -1.000000000000000000 ) ) ;
#864 = CARTESIAN_POINT ( 'NONE',  ( -3.756430356249996549, 26.67812499938548854, 6.831223922626973533 ) ) ;
#865 = AXIS2_PLACEMENT_3D ( 'NONE', #18096, #5921, #4344 ) ;
#866 = CARTESIAN_POINT ( 'NONE',  ( 1.071796769724492782, 26.44240381056766509, 4.999999999999989342 ) ) ;
#867 = CARTESIAN_POINT ( 'NONE',  ( 3.756430356250002323, 28.25312499938548783, 11.16877607737301226 ) ) ;
#868 = CARTESIAN_POINT ( 'NONE',  ( -29.07785765677936851, -9.610428525060582317, 1.000000000000000000 ) ) ;
#869 = AXIS2_PLACEMENT_3D ( 'NONE', #5265, #13243, #18616 ) ;
#870 = DIRECTION ( 'NONE',  ( -0.000000000000000000, -0.000000000000000000, 1.000000000000000000 ) ) ;
#871 = SHAPE_REPRESENTATION_RELATIONSHIP ( 'NONE' , 'NONE' ,  #23343, #13495 ) ;
#872 = CARTESIAN_POINT ( 'NONE',  ( 16.57281518405975262, 22.22966943355206126, 6.690598923241487306 ) ) ;
#873 = CARTESIAN_POINT ( 'NONE',  ( 0.000000000000000000, 0.000000000000000000, -6.500000000000000000 ) ) ;
#874 = CARTESIAN_POINT ( 'NONE',  ( 1.878215178125000939, 25.51562499938548356, 12.25316411605952283 ) ) ;
#875 = DIRECTION ( 'NONE',  ( 0.000000000000000000, 0.000000000000000000, 1.000000000000000000 ) ) ;
#876 = CARTESIAN_POINT ( 'NONE',  ( 15.00834143068450999, 20.66519568017682573, 8.999999999999992895 ) ) ;
#877 = CARTESIAN_POINT ( 'NONE',  ( 19.76811771667562567, 17.11192033871618534, 12.25316411605952283 ) ) ;
#878 = VECTOR ( 'NONE', #2181, 1000.000000000000000 ) ;
#879 = CYLINDRICAL_SURFACE ( 'NONE', #12623, 4.000000000000000000 ) ;
#880 = CYLINDRICAL_SURFACE ( 'NONE', #7552, 0.5000000000000000000 ) ;
#881 = CARTESIAN_POINT ( 'NONE',  ( 1.878215178125004048, 27.46562499938548640, 5.746835883940462963 ) ) ;
#882 = AXIS2_PLACEMENT_3D ( 'NONE', #14642, #16737, #24706 ) ;
#883 = CARTESIAN_POINT ( 'NONE',  ( -3.469446951953614189E-15, -30.00000000000000355, 4.999999999999992006 ) ) ;
#884 = CARTESIAN_POINT ( 'NONE',  ( -3.999999999999996447, 25.65624999877097068, 11.30940107675849404 ) ) ;
#885 = CARTESIAN_POINT ( 'NONE',  ( 4.000000000000003553, 25.39374999877096784, 8.999999999999992895 ) ) ;
#886 = ORIENTED_EDGE ( 'NONE', *, *, #2903, .T. ) ;
#887 = CARTESIAN_POINT ( 'NONE',  ( -25.75859848311247902, 16.66421332384710752, -6.500000000000000000 ) ) ;
#888 = CARTESIAN_POINT ( 'NONE',  ( -3.999999999999996003, 27.83124999877096784, 6.690598923241487306 ) ) ;
#889 = CARTESIAN_POINT ( 'NONE',  ( 1.878215178124995832, -27.99062499938548143, 5.746835883940462963 ) ) ;
#890 = ADVANCED_FACE ( 'NONE', ( #11377 ), #19355, .T. ) ;
#892 = ORIENTED_EDGE ( 'NONE', *, *, #8937, .F. ) ;
#891 = CARTESIAN_POINT ( 'NONE',  ( -1.071796769724487230, 25.31740381056767220, 12.99999999999999467 ) ) ;
#893 = DIRECTION ( 'NONE',  ( -0.000000000000000000, 0.000000000000000000, 1.000000000000000000 ) ) ;
#894 = ADVANCED_FACE ( 'NONE', ( #19093 ), #20431, .F. ) ;
#895 = EDGE_LOOP ( 'NONE', ( #13145, #10145, #12923, #16753 ) ) ;
#896 = CARTESIAN_POINT ( 'NONE',  ( 1.878215178124995832, -26.64062499938548711, 5.746835883940462963 ) ) ;
#897 = ORIENTED_EDGE ( 'NONE', *, *, #8841, .F. ) ;
#898 = ORIENTED_EDGE ( 'NONE', *, *, #3464, .T. ) ;
#899 = DIRECTION ( 'NONE',  ( 1.000000000000000000, 0.000000000000000000, 0.000000000000000000 ) ) ;
#900 = EDGE_CURVE ( 'NONE', #1141, #6126, #5120, .T. ) ;
#901 = CIRCLE ( 'NONE', #10903, 0.5000000000000009992 ) ;
#902 = CARTESIAN_POINT ( 'NONE',  ( -3.756430356249994773, 28.17812499938548854, 8.999999999999992895 ) ) ;
#903 = VECTOR ( 'NONE', #4470, 1000.000000000000000 ) ;
#904 = DIRECTION ( 'NONE',  ( 0.000000000000000000, 0.000000000000000000, 1.000000000000000000 ) ) ;
#905 =( BOUNDED_CURVE ( )  B_SPLINE_CURVE ( 2, ( #836, #22811, #4886, #22547, #12860, #20838, #2928, #10889, #5157 ),
 .UNSPECIFIED., .F., .F. ) 
 B_SPLINE_CURVE_WITH_KNOTS ( ( 3, 2, 2, 2, 3 ),
 ( 0.6250000000000000000, 0.6333333333333333037, 0.6500000000000000222, 0.6666666666666666297, 0.6750000000000000444 ),
 .UNSPECIFIED. ) 
 CURVE ( )  GEOMETRIC_REPRESENTATION_ITEM ( )  RATIONAL_B_SPLINE_CURVE ( ( 0.9330127018922194093, 0.9330127018922194093, 1.000000000000000000, 0.8660254037844387076, 1.000000000000000000, 0.8660254037844387076, 1.000000000000000000, 0.9330127018922189652, 0.9330127018922194093 ) ) 
 REPRESENTATION_ITEM ( '' )  );
#906 = VECTOR ( 'NONE', #5433, 1000.000000000000000 ) ;
#907 = EDGE_CURVE ( 'NONE', #21795, #24486, #23214, .T. ) ;
#908 = CARTESIAN_POINT ( 'NONE',  ( -3.756430356249995661, -6.831223922626973533, 1.790624999385484806 ) ) ;
#909 = CARTESIAN_POINT ( 'NONE',  ( 21.21320343559646915, 21.21320343559638744, 12.99999999999999289 ) ) ;
#910 =( BOUNDED_CURVE ( )  B_SPLINE_CURVE ( 2, ( #13594, #7704, #19208, #23776, #5349, #9288, #7824, #17391, #1829 ),
 .UNSPECIFIED., .F., .F. ) 
 B_SPLINE_CURVE_WITH_KNOTS ( ( 3, 2, 2, 2, 3 ),
 ( 0.4750000000000000333, 0.4833333333333333370, 0.5000000000000000000, 0.5166666666666667185, 0.5250000000000000222 ),
 .UNSPECIFIED. ) 
 CURVE ( )  GEOMETRIC_REPRESENTATION_ITEM ( )  RATIONAL_B_SPLINE_CURVE ( ( 0.9330127018922194093, 0.9330127018922196314, 1.000000000000000000, 0.8660254037844387076, 1.000000000000000000, 0.8660254037844387076, 1.000000000000000000, 0.9330127018922194093, 0.9330127018922194093 ) ) 
 REPRESENTATION_ITEM ( '' )  );
#911 = CARTESIAN_POINT ( 'NONE',  ( -1.878215178124998497, 27.69062499938548427, 12.25316411605951927 ) ) ;
#912 = CARTESIAN_POINT ( 'NONE',  ( 16.91752973988819164, 22.57438398938050028, 8.999999999999992895 ) ) ;
#913 = CARTESIAN_POINT ( 'NONE',  ( 0.000000000000000000, 0.000000000000000000, 19.50000000000000000 ) ) ;
#914 = CARTESIAN_POINT ( 'NONE',  ( 3.756430356250002323, 29.60312499938548569, 11.16877607737301403 ) ) ;
#915 = DIRECTION ( 'NONE',  ( 0.000000000000000000, -0.000000000000000000, -1.000000000000000000 ) ) ;
#916 = CARTESIAN_POINT ( 'NONE',  ( 22.71619846896431483, 19.59662171127745367, 12.34935938736417071 ) ) ;
#917 = DIRECTION ( 'NONE',  ( 0.8660254037844397068, 0.000000000000000000, -0.4999999999999983347 ) ) ;
#918 = CARTESIAN_POINT ( 'NONE',  ( 0.5000000000000000000, -2.999999999999999556, 19.50000000000000000 ) ) ;
#919 = CARTESIAN_POINT ( 'NONE',  ( -3.756430356250004099, -27.99062499938548498, 6.831223922626973533 ) ) ;
#920 = VECTOR ( 'NONE', #11822, 1000.000000000000000 ) ;
#921 = LINE ( 'NONE', #7050, #24021 ) ;
#922 = AXIS2_PLACEMENT_3D ( 'NONE', #15072, #2899, #7219 ) ;
#923 = DIRECTION ( 'NONE',  ( -0.000000000000000000, -0.000000000000000000, 1.000000000000000000 ) ) ;
#924 = CARTESIAN_POINT ( 'NONE',  ( 4.648177544792955347E-16, 26.68750000000000711, 12.99999999999999289 ) ) ;
#925 = EDGE_CURVE ( 'NONE', #2876, #7537, #14389, .T. ) ;
#926 = CARTESIAN_POINT ( 'NONE',  ( 1.057460391440397258E-14, -28.71250000000000213, 4.999999999999992006 ) ) ;
#927 = ORIENTED_EDGE ( 'NONE', *, *, #22382, .F. ) ;
#928 = LINE ( 'NONE', #2364, #18787 ) ;
#930 = VERTEX_POINT ( 'NONE', #7833 ) ;
#929 = CARTESIAN_POINT ( 'NONE',  ( 23.96296185032708337, 19.82388608118420237, -6.500000000000000000 ) ) ;
#931 = CIRCLE ( 'NONE', #15119, 0.5000000000000019984 ) ;
#932 = EDGE_CURVE ( 'NONE', #17398, #3560, #135, .T. ) ;
#933 = VERTEX_POINT ( 'NONE', #17905 ) ;
#934 = ORIENTED_EDGE ( 'NONE', *, *, #15408, .T. ) ;
#935 = ORIENTED_EDGE ( 'NONE', *, *, #9732, .T. ) ;
#936 = ORIENTED_EDGE ( 'NONE', *, *, #14930, .F. ) ;
#937 = CARTESIAN_POINT ( 'NONE',  ( 0.000000000000000000, 0.000000000000000000, -6.500000000000000000 ) ) ;
#938 = CIRCLE ( 'NONE', #13461, 31.10000000000000142 ) ;
#939 = VERTEX_POINT ( 'NONE', #5622 ) ;
#940 = CARTESIAN_POINT ( 'NONE',  ( 26.00000000000000711, 3.184081677783118980E-15, 20.00000000000000000 ) ) ;
#941 = CARTESIAN_POINT ( 'NONE',  ( -3.756430356249997438, 28.66562499938548569, 11.16877607737301048 ) ) ;
#942 = AXIS2_PLACEMENT_3D ( 'NONE', #11479, #21672, #15167 ) ;
#943 = CIRCLE ( 'NONE', #12616, 0.4999999999999999445 ) ;
#944 = ADVANCED_FACE ( 'NONE', ( #7714 ), #1569, .T. ) ;
#945 = CARTESIAN_POINT ( 'NONE',  ( -3.756430356249996994, -8.999999999999992895, 0.3656249993854825409 ) ) ;
#946 = FILL_AREA_STYLE_COLOUR ( '', #5841 ) ;
#947 = CARTESIAN_POINT ( 'NONE',  ( 18.11727402765218287, 23.42966878357085037, 6.831223922626973533 ) ) ;
#948 = AXIS2_PLACEMENT_3D ( 'NONE', #2206, #241, #4289 ) ;
#949 = CARTESIAN_POINT ( 'NONE',  ( -1.878215178124995832, 26.75312499938548783, 5.746835883940462963 ) ) ;
#950 = CARTESIAN_POINT ( 'NONE',  ( -20.67279826512042007, -15.85973458909327150, 20.00001200000000168 ) ) ;
#951 = CARTESIAN_POINT ( 'NONE',  ( 1.878215178125004048, -5.746835883940462963, 3.365624999385481875 ) ) ;
#952 = LINE ( 'NONE', #11007, #17147 ) ;
#953 = CARTESIAN_POINT ( 'NONE',  ( -3.999999999999997335, -11.30940107675849404, 3.862499999999996714 ) ) ;
#954 = CARTESIAN_POINT ( 'NONE',  ( 20.26302869750798408, 20.26302869750790947, 4.999999999999992006 ) ) ;
#955 = CARTESIAN_POINT ( 'NONE',  ( -8.217531866530787710, 29.99470236596041772, 1.000000000000000000 ) ) ;
#956 = CARTESIAN_POINT ( 'NONE',  ( 0.000000000000000000, 0.000000000000000000, 1.000000000000000000 ) ) ;
#957 = CARTESIAN_POINT ( 'NONE',  ( 2.000000000000003997, 27.71874999877097068, 5.535898384862238508 ) ) ;
#958 = AXIS2_PLACEMENT_3D ( 'NONE', #19324, #9263, #17252 ) ;
#959 = DIRECTION ( 'NONE',  ( 1.000000000000000000, 0.000000000000000000, 0.000000000000000000 ) ) ;
#960 = ORIENTED_EDGE ( 'NONE', *, *, #11857, .T. ) ;
#961 = VERTEX_POINT ( 'NONE', #19858 ) ;
#962 = VERTEX_POINT ( 'NONE', #2085 ) ;
#963 = PLANE ( 'NONE',  #13721 ) ;
#964 = ORIENTED_EDGE ( 'NONE', *, *, #14508, .T. ) ;
#965 = CARTESIAN_POINT ( 'NONE',  ( -1.878215178125004048, -25.32812499938548356, 5.746835883940462963 ) ) ;
#966 = ORIENTED_EDGE ( 'NONE', *, *, #11818, .F. ) ;
#967 = PLANE ( 'NONE',  #8845 ) ;
#968 = CIRCLE ( 'NONE', #10980, 0.5000000000000004441 ) ;
#969 = ORIENTED_EDGE ( 'NONE', *, *, #11626, .T. ) ;
#970 = CARTESIAN_POINT ( 'NONE',  ( 3.999999999999996447, -29.27500000000000213, 8.999999999999992895 ) ) ;
#971 = CARTESIAN_POINT ( 'NONE',  ( -1.878215178124998497, 29.04062499938548569, 12.25316411605951927 ) ) ;
#972 = CARTESIAN_POINT ( 'NONE',  ( 17.74838020778238246, 20.57680733252850303, 12.46410161513774639 ) ) ;
#973 = AXIS2_PLACEMENT_3D ( 'NONE', #20831, #5152, #18742 ) ;
#974 = DIRECTION ( 'NONE',  ( 0.000000000000000000, 0.000000000000000000, -1.000000000000000000 ) ) ;
#975 = CARTESIAN_POINT ( 'NONE',  ( 0.000000000000000000, 0.000000000000000000, -6.500000000000000000 ) ) ;
#976 = CARTESIAN_POINT ( 'NONE',  ( 21.04090992281141581, 18.38471254485196837, 12.25316411605952283 ) ) ;
#977 = DIRECTION ( 'NONE',  ( -0.000000000000000000, 0.000000000000000000, 1.000000000000000000 ) ) ;
#978 = CARTESIAN_POINT ( 'NONE',  ( 2.000000000000003997, 26.87500000000000355, 5.535898384862238508 ) ) ;
#979 = CARTESIAN_POINT ( 'NONE',  ( 20.08631576820957321, 17.43011839025013288, 12.25316411605952283 ) ) ;
#980 = DIRECTION ( 'NONE',  ( 0.000000000000000000, 0.000000000000000000, 1.000000000000000000 ) ) ;
#981 = ORIENTED_EDGE ( 'NONE', *, *, #3136, .T. ) ;
#982 = CARTESIAN_POINT ( 'NONE',  ( 2.000000000000000000, 25.76874999877097139, 12.46410161513774817 ) ) ;
#983 = CARTESIAN_POINT ( 'NONE',  ( -3.735045420075836212E-15, -27.95312499938548001, 4.662447845253954171 ) ) ;
#984 = VECTOR ( 'NONE', #20472, 1000.000000000000000 ) ;
#985 = DIRECTION ( 'NONE',  ( -0.000000000000000000, -0.000000000000000000, 1.000000000000000000 ) ) ;
#986 = CARTESIAN_POINT ( 'NONE',  ( -1.999999999999995781, 29.14374999877096784, 5.535898384862237620 ) ) ;
#987 = LINE ( 'NONE', #19022, #11275 ) ;
#989 = ORIENTED_EDGE ( 'NONE', *, *, #6792, .F. ) ;
#988 = CARTESIAN_POINT ( 'NONE',  ( 3.756430356250004099, -6.831223922626973533, 0.1781249993854828739 ) ) ;
#990 = VERTEX_POINT ( 'NONE', #9919 ) ;
#991 = DIRECTION ( 'NONE',  ( 0.000000000000000000, -1.000000000000000000, 0.000000000000000000 ) ) ;
#992 = ADVANCED_FACE ( 'NONE', ( #17662 ), #3650, .T. ) ;
#993 = LINE ( 'NONE', #11166, #22178 ) ;
#994 = ORIENTED_EDGE ( 'NONE', *, *, #24626, .F. ) ;
#995 = CARTESIAN_POINT ( 'NONE',  ( -3.999999999999996447, 25.67500000000000071, 8.999999999999992895 ) ) ;
#996 = LINE ( 'NONE', #14734, #15134 ) ;
#997 = CARTESIAN_POINT ( 'NONE',  ( -3.897863563850083146, -30.85476721088024021, 1.000000000000000000 ) ) ;
#998 = EDGE_CURVE ( 'NONE', #132, #22067, #11624, .T. ) ;
#999 = DIRECTION ( 'NONE',  ( 0.000000000000000000, 0.000000000000000000, 1.000000000000000000 ) ) ;
#1000 = CARTESIAN_POINT ( 'NONE',  ( -1.878215178124999829, 29.04062499938549280, 12.25316411605951927 ) ) ;
#1001 = EDGE_CURVE ( 'NONE', #24168, #16234, #15818, .T. ) ;
#1002 = CIRCLE ( 'NONE', #15623, 0.4999999999999998335 ) ;
#1003 = CARTESIAN_POINT ( 'NONE',  ( 3.959305671612554781E-15, 30.00000000000000355, 12.99999999999999289 ) ) ;
#1004 = DIRECTION ( 'NONE',  ( -1.000000000000000000, 0.000000000000000000, 0.000000000000000000 ) ) ;
#1005 = ADVANCED_FACE ( 'NONE', ( #19741 ), #11764, .T. ) ;
#1006 = DIRECTION ( 'NONE',  ( -0.000000000000000000, -0.000000000000000000, 1.000000000000000000 ) ) ;
#1007 = CARTESIAN_POINT ( 'NONE',  ( 27.25313774936409317, -14.98253926456347074, -6.500000000000000000 ) ) ;
#1008 = CARTESIAN_POINT ( 'NONE',  ( 1.878215178125000939, 27.31562499938548427, 12.25316411605952283 ) ) ;
#1009 = CARTESIAN_POINT ( 'NONE',  ( 21.76563060752939549, 16.10877635803693764, 6.690598923241489970 ) ) ;
#1010 = CARTESIAN_POINT ( 'NONE',  ( 19.35704813498177046, 16.52862101023551844, 12.46410161513774817 ) ) ;
#1011 = CARTESIAN_POINT ( 'NONE',  ( 20.51057983692150444, 17.85438245896205700, 5.746835883940462963 ) ) ;
#1012 = CARTESIAN_POINT ( 'NONE',  ( -14.48253926456356666, -27.25313774936403988, 1.000000000000000000 ) ) ;
#1013 = CARTESIAN_POINT ( 'NONE',  ( -3.756430356249996994, 26.71562499938548285, 8.999999999999992895 ) ) ;
#1014 = CARTESIAN_POINT ( 'NONE',  ( -15.41874213889422940, -27.00874656207295743, 1.000000000000000000 ) ) ;
#1015 =( BOUNDED_SURFACE ( )  B_SPLINE_SURFACE ( 1, 2, ( 
 ( #20359, #23917, #22212, #24040, #19970, #12521, #4299, #10557, #20237, #8483, #12270, #2334, #7960, #4030, #8345, #24161, #25873, #15946, #11996, #2075, #6121, #14105, #22069, #10417, #4158, #12134, #20111, #2215, #10172, #16469, #14242, #22336, #10294, #374, #16333, #6387, #14377, #24545, #18556, #18669, #2717, #10807, #19051, #22987, #4931, #2978, #20635, #10946, #21149, #3220, #1136, #8725, #10680, #7159, #13051, #18937, #16856, #22735, #637, #755, #20891, #8605, #20761, #5072, #25073, #888, #1021, #16712, #4814, #24940, #12914, #16586, #13179, #6630, #14622, #16975, #8995, #24821, #3108, #5200, #12789, #21029, #2840, #6898, #12664, #11073, #22602, #9109, #17098, #14881, #4685, #24687, #7020, #22856, #6772, #14757, #15150, #15006, #18800, #8872, #23118, #7886, #3355, #13298, #17836, #2147, #21890, #21272, #188, #11330, #16015, #6182, #11938, #19908, #2007, #15386, #14171, #9977, #3973, #6062, #17968 ),
 ( #24100, #11192, #5935, #19313, #12064, #23981, #58, #23359, #5448, #14046, #15876, #1408, #9383, #25805, #10112, #8031, #17362, #8158, #25327, #22011, #22143, #4089, #20043, #18113, #13440, #19172, #16139, #1269, #9253, #17241, #21410, #25211, #5318, #7291, #15267, #23235, #7407, #23848, #3491, #13920, #11462, #19793, #1890, #9854, #25768, #1856, #7848, #15589, #17680, #19760, #9554, #1972, #5894, #9938, #17923, #15714, #13880, #13620, #1723, #9698, #15979, #2102, #21853, #15833, #14, #23559, #19999, #3936, #11904, #11783, #5640, #9817, #14130, #17802, #21585, #3665, #23942, #17543, #19872, #6025, #4052, #21977, #7990, #14007, #25518, #12021, #24064, #10070, #18071, #11643, #153, #19618, #25649, #7605, #23806, #7729, #23677, #5754, #8124, #6146, #16099, #13741, #22096, #21718, #4185, #3803, #19489, #1585, #12691, #4569, #10706, #16609, #18446, #16364, #22760, #780, #4719, #8245, #8631, #22632, #12162 ) ),
 .UNSPECIFIED., .F., .F., .T. ) 
 B_SPLINE_SURFACE_WITH_KNOTS ( ( 2, 2 ),
 ( 3, 2, 2, 2, 2, 2, 2, 2, 2, 2, 2, 2, 2, 2, 2, 2, 2, 2, 2, 2, 2, 2, 2, 2, 2, 2, 2, 2, 2, 2, 2, 2, 2, 2, 2, 2, 2, 2, 2, 2, 2, 2, 2, 2, 2, 2, 2, 2, 2, 2, 2, 2, 2, 2, 2, 2, 2, 2, 2, 2, 3 ),
 ( 0.000000000000000000, 1.000000000000000000 ),
 ( 0.000000000000000000, 0.01666666666666666644, 0.03333333333333333287, 0.05000000000000000278, 0.06666666666666666574, 0.08333333333333332871, 0.1000000000000000056, 0.1166666666666666685, 0.1333333333333333315, 0.1499999999999999944, 0.1666666666666666574, 0.1833333333333333204, 0.2000000000000000111, 0.2166666666666666741, 0.2333333333333333370, 0.2500000000000000000, 0.2666666666666666630, 0.2833333333333333259, 0.2999999999999999889, 0.3166666666666666519, 0.3333333333333333148, 0.3499999999999999778, 0.3666666666666666408, 0.3833333333333333592, 0.4000000000000000222, 0.4166666666666666852, 0.4333333333333333481, 0.4500000000000000111, 0.4666666666666666741, 0.4833333333333333370, 0.5000000000000000000, 0.5166666666666667185, 0.5333333333333333259, 0.5500000000000000444, 0.5666666666666666519, 0.5833333333333333703, 0.5999999999999999778, 0.6166666666666666963, 0.6333333333333333037, 0.6500000000000000222, 0.6666666666666666297, 0.6833333333333333481, 0.6999999999999999556, 0.7166666666666666741, 0.7333333333333332815, 0.7500000000000000000, 0.7666666666666667185, 0.7833333333333333259, 0.8000000000000000444, 0.8166666666666666519, 0.8333333333333333703, 0.8499999999999999778, 0.8666666666666666963, 0.8833333333333333037, 0.9000000000000000222, 0.9166666666666666297, 0.9333333333333333481, 0.9499999999999999556, 0.9666666666666666741, 0.9833333333333332815, 1.000000000000000000 ),
 .UNSPECIFIED. ) 
 GEOMETRIC_REPRESENTATION_ITEM ( )  RATIONAL_B_SPLINE_SURFACE ( (
 ( 1.000000000000000000, 0.8660254037844387076, 1.000000000000000000, 0.8660254037844387076, 1.000000000000000000, 0.8660254037844387076, 1.000000000000000000, 0.8660254037844387076, 1.000000000000000000, 0.8660254037844387076, 1.000000000000000000, 0.8660254037844387076, 1.000000000000000000, 0.8660254037844387076, 1.000000000000000000, 0.8660254037844387076, 1.000000000000000000, 0.8660254037844387076, 1.000000000000000000, 0.8660254037844387076, 1.000000000000000000, 0.8660254037844387076, 1.000000000000000000, 0.8660254037844387076, 1.000000000000000000, 0.8660254037844387076, 1.000000000000000000, 0.8660254037844387076, 1.000000000000000000, 0.8660254037844387076, 1.000000000000000000, 0.8660254037844387076, 1.000000000000000000, 0.8660254037844387076, 1.000000000000000000, 0.8660254037844387076, 1.000000000000000000, 0.8660254037844387076, 1.000000000000000000, 0.8660254037844387076, 1.000000000000000000, 0.8660254037844387076, 1.000000000000000000, 0.8660254037844387076, 1.000000000000000000, 0.8660254037844387076, 1.000000000000000000, 0.8660254037844387076, 1.000000000000000000, 0.8660254037844387076, 1.000000000000000000, 0.8660254037844387076, 1.000000000000000000, 0.8660254037844387076, 1.000000000000000000, 0.8660254037844387076, 1.000000000000000000, 0.8660254037844387076, 1.000000000000000000, 0.8660254037844387076, 1.000000000000000000, 0.8660254037844387076, 1.000000000000000000, 0.8660254037844387076, 1.000000000000000000, 0.8660254037844387076, 1.000000000000000000, 0.8660254037844387076, 1.000000000000000000, 0.8660254037844387076, 1.000000000000000000, 0.8660254037844387076, 1.000000000000000000, 0.8660254037844387076, 1.000000000000000000, 0.8660254037844387076, 1.000000000000000000, 0.8660254037844387076, 1.000000000000000000, 0.8660254037844387076, 1.000000000000000000, 0.8660254037844387076, 1.000000000000000000, 0.8660254037844387076, 1.000000000000000000, 0.8660254037844387076, 1.000000000000000000, 0.8660254037844387076, 1.000000000000000000, 0.8660254037844387076, 1.000000000000000000, 0.8660254037844387076, 1.000000000000000000, 0.8660254037844387076, 1.000000000000000000, 0.8660254037844387076, 1.000000000000000000, 0.8660254037844387076, 1.000000000000000000, 0.8660254037844387076, 1.000000000000000000, 0.8660254037844387076, 1.000000000000000000, 0.8660254037844387076, 1.000000000000000000, 0.8660254037844387076, 1.000000000000000000, 0.8660254037844387076, 1.000000000000000000, 0.8660254037844387076, 1.000000000000000000, 0.8660254037844387076, 1.000000000000000000, 0.8660254037844387076, 1.000000000000000000, 0.8660254037844387076, 1.000000000000000000, 0.8660254037844387076, 1.000000000000000000, 0.8660254037844387076, 1.000000000000000000),
 ( 1.000000000000000000, 0.8660254037844387076, 1.000000000000000000, 0.8660254037844387076, 1.000000000000000000, 0.8660254037844387076, 1.000000000000000000, 0.8660254037844387076, 1.000000000000000000, 0.8660254037844387076, 1.000000000000000000, 0.8660254037844387076, 1.000000000000000000, 0.8660254037844387076, 1.000000000000000000, 0.8660254037844387076, 1.000000000000000000, 0.8660254037844387076, 1.000000000000000000, 0.8660254037844387076, 1.000000000000000000, 0.8660254037844387076, 1.000000000000000000, 0.8660254037844387076, 1.000000000000000000, 0.8660254037844387076, 1.000000000000000000, 0.8660254037844387076, 1.000000000000000000, 0.8660254037844387076, 1.000000000000000000, 0.8660254037844387076, 1.000000000000000000, 0.8660254037844387076, 1.000000000000000000, 0.8660254037844387076, 1.000000000000000000, 0.8660254037844387076, 1.000000000000000000, 0.8660254037844387076, 1.000000000000000000, 0.8660254037844387076, 1.000000000000000000, 0.8660254037844387076, 1.000000000000000000, 0.8660254037844387076, 1.000000000000000000, 0.8660254037844387076, 1.000000000000000000, 0.8660254037844387076, 1.000000000000000000, 0.8660254037844387076, 1.000000000000000000, 0.8660254037844387076, 1.000000000000000000, 0.8660254037844387076, 1.000000000000000000, 0.8660254037844387076, 1.000000000000000000, 0.8660254037844387076, 1.000000000000000000, 0.8660254037844387076, 1.000000000000000000, 0.8660254037844387076, 1.000000000000000000, 0.8660254037844387076, 1.000000000000000000, 0.8660254037844387076, 1.000000000000000000, 0.8660254037844387076, 1.000000000000000000, 0.8660254037844387076, 1.000000000000000000, 0.8660254037844387076, 1.000000000000000000, 0.8660254037844387076, 1.000000000000000000, 0.8660254037844387076, 1.000000000000000000, 0.8660254037844387076, 1.000000000000000000, 0.8660254037844387076, 1.000000000000000000, 0.8660254037844387076, 1.000000000000000000, 0.8660254037844387076, 1.000000000000000000, 0.8660254037844387076, 1.000000000000000000, 0.8660254037844387076, 1.000000000000000000, 0.8660254037844387076, 1.000000000000000000, 0.8660254037844387076, 1.000000000000000000, 0.8660254037844387076, 1.000000000000000000, 0.8660254037844387076, 1.000000000000000000, 0.8660254037844387076, 1.000000000000000000, 0.8660254037844387076, 1.000000000000000000, 0.8660254037844387076, 1.000000000000000000, 0.8660254037844387076, 1.000000000000000000, 0.8660254037844387076, 1.000000000000000000, 0.8660254037844387076, 1.000000000000000000, 0.8660254037844387076, 1.000000000000000000, 0.8660254037844387076, 1.000000000000000000, 0.8660254037844387076, 1.000000000000000000, 0.8660254037844387076, 1.000000000000000000, 0.8660254037844387076, 1.000000000000000000) ) ) 
 REPRESENTATION_ITEM ( '' )  SURFACE ( )  );
#1016 =( GEOMETRIC_REPRESENTATION_CONTEXT ( 3 ) GLOBAL_UNCERTAINTY_ASSIGNED_CONTEXT ( ( #1041 ) ) GLOBAL_UNIT_ASSIGNED_CONTEXT ( ( #6492, #1118, #6050 ) ) REPRESENTATION_CONTEXT ( 'NONE', 'WORKASPACE' ) );
#1017 = CARTESIAN_POINT ( 'NONE',  ( 21.38789795289476103, 16.07550319697594432, 8.999999999999992895 ) ) ;
#1018 = DIRECTION ( 'NONE',  ( -0.000000000000000000, -0.000000000000000000, 1.000000000000000000 ) ) ;
#1019 = ORIENTED_EDGE ( 'NONE', *, *, #4892, .T. ) ;
#1020 = DIRECTION ( 'NONE',  ( -0.000000000000000000, -1.000000000000000000, -0.000000000000000000 ) ) ;
#1021 = CARTESIAN_POINT ( 'NONE',  ( -3.999999999999996447, 27.86874999877096570, 8.999999999999992895 ) ) ;
#1022 = CARTESIAN_POINT ( 'NONE',  ( 3.999999999999996447, -25.22500000000000142, 8.999999999999992895 ) ) ;
#1024 = ORIENTED_EDGE ( 'NONE', *, *, #18629, .T. ) ;
#1023 = DIRECTION ( 'NONE',  ( 0.000000000000000000, 0.000000000000000000, 1.000000000000000000 ) ) ;
#1025 = CARTESIAN_POINT ( 'NONE',  ( 18.05905254985559338, 19.57480207770756664, 12.99999999999999467 ) ) ;
#1026 = ORIENTED_EDGE ( 'NONE', *, *, #13707, .T. ) ;
#1027 = CARTESIAN_POINT ( 'NONE',  ( -3.756430356250002323, -28.70312499938548356, 11.16877607737301226 ) ) ;
#1028 = ORIENTED_EDGE ( 'NONE', *, *, #14569, .T. ) ;
#1029 = ORIENTED_EDGE ( 'NONE', *, *, #11563, .T. ) ;
#1030 = CARTESIAN_POINT ( 'NONE',  ( 20.28164449898397947, 22.10686971680496882, 5.204870533884474959 ) ) ;
#1031 = CARTESIAN_POINT ( 'NONE',  ( 3.756430356250004543, 28.81562499938548783, 11.16877607737301226 ) ) ;
#1032 = ADVANCED_FACE ( 'NONE', ( #13862, #15695 ), #16085, .F. ) ;
#1033 = LINE ( 'NONE', #20513, #7659 ) ;
#1034 = CARTESIAN_POINT ( 'NONE',  ( -1.878215178124995832, -5.746835883940462963, 4.003124999385484273 ) ) ;
#1035 = EDGE_CURVE ( 'NONE', #18677, #23884, #21970, .T. ) ;
#1036 = CARTESIAN_POINT ( 'NONE',  ( -3.100818392631252696, 38.96327129008100343, 4.412772063012910806 ) ) ;
#1037 = CARTESIAN_POINT ( 'NONE',  ( -1.878215178124998497, 27.24062499938548498, 12.25316411605951927 ) ) ;
#1038 = ADVANCED_FACE ( 'NONE', ( #8228 ), #2609, .F. ) ;
#1039 = DIRECTION ( 'NONE',  ( 1.000000000000000000, 0.000000000000000000, 0.000000000000000000 ) ) ;
#1040 = UNCERTAINTY_MEASURE_WITH_UNIT (LENGTH_MEASURE( 1.000000000000000082E-05 ), #9039, 'distance_accuracy_value', 'NONE');
#1041 = UNCERTAINTY_MEASURE_WITH_UNIT (LENGTH_MEASURE( 1.000000000000000082E-05 ), #6492, 'distance_accuracy_value', 'NONE');
#1042 = CARTESIAN_POINT ( 'NONE',  ( 1.878215178125004048, 29.26562499938548356, 5.746835883940462963 ) ) ;
#1043 = CARTESIAN_POINT ( 'NONE',  ( -5.827558883615604479, 30.54913349766230724, -6.500000000000000000 ) ) ;
#1044 = LINE ( 'NONE', #17127, #12204 ) ;
#1045 = DIRECTION ( 'NONE',  ( 0.000000000000000000, 0.000000000000000000, 1.000000000000000000 ) ) ;
#1046 = CARTESIAN_POINT ( 'NONE',  ( -3.735045420075836212E-15, -28.06562499938548427, 4.662447845253954171 ) ) ;
#1047 = CARTESIAN_POINT ( 'NONE',  ( 18.55713358789543932, 21.38556071264155634, 5.535898384862237620 ) ) ;
#1048 = CARTESIAN_POINT ( 'NONE',  ( 3.834746474454188013E-15, 27.75624999877096855, 4.999999999999992006 ) ) ;
#1049 = CARTESIAN_POINT ( 'NONE',  ( -1.999999999999995781, 25.99374999877096926, 5.535898384862237620 ) ) ;
#1050 = DIRECTION ( 'NONE',  ( 0.000000000000000000, 0.000000000000000000, 1.000000000000000000 ) ) ;
#1051 = VERTEX_POINT ( 'NONE', #12533 ) ;
#1052 = CARTESIAN_POINT ( 'NONE',  ( -21.28941499438192864, 22.67092431280617859, -6.500000000000000000 ) ) ;
#1054 = EDGE_LOOP ( 'NONE', ( #15352, #6511, #21097, #21569 ) ) ;
#1053 = LINE ( 'NONE', #8910, #8748 ) ;
#1055 = VERTEX_POINT ( 'NONE', #16202 ) ;
#1056 = EDGE_LOOP ( 'NONE', ( #14111, #12304, #8307, #3326 ) ) ;
#1057 = ORIENTED_EDGE ( 'NONE', *, *, #1504, .F. ) ;
#1058 = ORIENTED_EDGE ( 'NONE', *, *, #2728, .F. ) ;
#1059 = CARTESIAN_POINT ( 'NONE',  ( -1.071796769724498999, -27.60759618943233207, 12.99999999999998757 ) ) ;
#1060 = CARTESIAN_POINT ( 'NONE',  ( 0.000000000000000000, 0.000000000000000000, -6.500000000000000000 ) ) ;
#1061 = ORIENTED_EDGE ( 'NONE', *, *, #5924, .T. ) ;
#1062 = CARTESIAN_POINT ( 'NONE',  ( 3.756430356250003211, 27.99062499938548498, 6.831223922626973533 ) ) ;
#1063 =( BOUNDED_SURFACE ( )  B_SPLINE_SURFACE ( 1, 2, ( 
 ( #4499, #12474, #18900, #2547, #4375, #12621, #12354, #10517, #18514, #718, #982, #601, #16550, #14846, #24780, #24255, #24509, #6591, #24638, #16670, #10766, #20594, #2680, #6726, #14718, #4778, #20723, #4895, #18755, #847, #8827, #6863, #12871, #11156, #21500, #11290, #17201, #15234, #13531, #5029, #25173, #22943, #11037, #23082, #11550, #16938, #23320, #23458, #9347, #23198, #21375, #9466, #19016, #13398, #15350, #3188, #5168, #19137, #24908, #21231, #19517, #13009, #7121, #9211, #7253, #1100, #25294, #7497, #13259, #3314, #15490, #20993, #6984, #15107, #3454, #5283, #17329, #11428, #14966, #9076, #3070, #17059, #5547, #19402, #7373, #3579, #25030, #8963, #19270, #1372, #13146, #5411, #21110, #1493, #1229, #17443, #25410, #13779, #8026, #21886, #9590, #21616, #23589, #11817, #25552, #10106, #13916, #13649, #15744, #23706, #4225, #5789, #25680, #53, #3699, #17712, #8155, #17576, #5670, #1887, #16135 ),
 ( #7883, #19655, #7637, #6179, #185, #11679, #24096, #9850, #15871, #14166, #25802, #22138, #9974, #1762, #9731, #17965, #21756, #16011, #3969, #15622, #7761, #3838, #19789, #17832, #18108, #11935, #23844, #5930, #19903, #12202, #2003, #23978, #6058, #14042, #22008, #1616, #4085, #12059, #20040, #2143, #445, #16259, #2658, #8414, #578, #12331, #10228, #24757, #24230, #6839, #20298, #18225, #18490, #8278, #6316, #307, #14550, #14823, #10346, #4476, #18729, #20698, #22795, #14312, #4872, #10620, #4610, #14692, #22274, #20172, #2392, #4354, #2273, #16403, #819, #22396, #16646, #18347, #22529, #12591, #12451, #24371, #20570, #2521, #8547, #6448, #14432, #10490, #20420, #16528, #24488, #6569, #18612, #8664, #8798, #699, #24613, #6698, #2779, #22672, #4759, #12728, #10742, #16787, #23397, #21179, #25488, #15806, #17276, #11366, #13477, #11495, #23265, #3641, #11753, #17511, #7574, #19732, #25241, #11227, #19345 ) ),
 .UNSPECIFIED., .F., .F., .F. ) 
 B_SPLINE_SURFACE_WITH_KNOTS ( ( 2, 2 ),
 ( 3, 2, 2, 2, 2, 2, 2, 2, 2, 2, 2, 2, 2, 2, 2, 2, 2, 2, 2, 2, 2, 2, 2, 2, 2, 2, 2, 2, 2, 2, 2, 2, 2, 2, 2, 2, 2, 2, 2, 2, 2, 2, 2, 2, 2, 2, 2, 2, 2, 2, 2, 2, 2, 2, 2, 2, 2, 2, 2, 2, 3 ),
 ( 0.000000000000000000, 1.000000000000000000 ),
 ( 0.000000000000000000, 0.01666666666666666644, 0.03333333333333333287, 0.05000000000000000278, 0.06666666666666666574, 0.08333333333333332871, 0.1000000000000000056, 0.1166666666666666685, 0.1333333333333333315, 0.1499999999999999944, 0.1666666666666666574, 0.1833333333333333204, 0.2000000000000000111, 0.2166666666666666741, 0.2333333333333333370, 0.2500000000000000000, 0.2666666666666666630, 0.2833333333333333259, 0.2999999999999999889, 0.3166666666666666519, 0.3333333333333333148, 0.3499999999999999778, 0.3666666666666666408, 0.3833333333333333592, 0.4000000000000000222, 0.4166666666666666852, 0.4333333333333333481, 0.4500000000000000111, 0.4666666666666666741, 0.4833333333333333370, 0.5000000000000000000, 0.5166666666666667185, 0.5333333333333333259, 0.5500000000000000444, 0.5666666666666666519, 0.5833333333333333703, 0.5999999999999999778, 0.6166666666666666963, 0.6333333333333333037, 0.6500000000000000222, 0.6666666666666666297, 0.6833333333333333481, 0.6999999999999999556, 0.7166666666666666741, 0.7333333333333332815, 0.7500000000000000000, 0.7666666666666667185, 0.7833333333333333259, 0.8000000000000000444, 0.8166666666666666519, 0.8333333333333333703, 0.8499999999999999778, 0.8666666666666666963, 0.8833333333333333037, 0.9000000000000000222, 0.9166666666666666297, 0.9333333333333333481, 0.9499999999999999556, 0.9666666666666666741, 0.9833333333333332815, 1.000000000000000000 ),
 .UNSPECIFIED. ) 
 GEOMETRIC_REPRESENTATION_ITEM ( )  RATIONAL_B_SPLINE_SURFACE ( (
 ( 1.000000000000000000, 0.8660254037844387076, 1.000000000000000000, 0.8660254037844387076, 1.000000000000000000, 0.8660254037844387076, 1.000000000000000000, 0.8660254037844387076, 1.000000000000000000, 0.8660254037844387076, 1.000000000000000000, 0.8660254037844387076, 1.000000000000000000, 0.8660254037844387076, 1.000000000000000000, 0.8660254037844387076, 1.000000000000000000, 0.8660254037844387076, 1.000000000000000000, 0.8660254037844387076, 1.000000000000000000, 0.8660254037844387076, 1.000000000000000000, 0.8660254037844387076, 1.000000000000000000, 0.8660254037844387076, 1.000000000000000000, 0.8660254037844387076, 1.000000000000000000, 0.8660254037844387076, 1.000000000000000000, 0.8660254037844387076, 1.000000000000000000, 0.8660254037844387076, 1.000000000000000000, 0.8660254037844387076, 1.000000000000000000, 0.8660254037844387076, 1.000000000000000000, 0.8660254037844387076, 1.000000000000000000, 0.8660254037844387076, 1.000000000000000000, 0.8660254037844387076, 1.000000000000000000, 0.8660254037844387076, 1.000000000000000000, 0.8660254037844387076, 1.000000000000000000, 0.8660254037844387076, 1.000000000000000000, 0.8660254037844387076, 1.000000000000000000, 0.8660254037844387076, 1.000000000000000000, 0.8660254037844387076, 1.000000000000000000, 0.8660254037844387076, 1.000000000000000000, 0.8660254037844387076, 1.000000000000000000, 0.8660254037844387076, 1.000000000000000000, 0.8660254037844387076, 1.000000000000000000, 0.8660254037844387076, 1.000000000000000000, 0.8660254037844387076, 1.000000000000000000, 0.8660254037844387076, 1.000000000000000000, 0.8660254037844387076, 1.000000000000000000, 0.8660254037844387076, 1.000000000000000000, 0.8660254037844387076, 1.000000000000000000, 0.8660254037844387076, 1.000000000000000000, 0.8660254037844387076, 1.000000000000000000, 0.8660254037844387076, 1.000000000000000000, 0.8660254037844387076, 1.000000000000000000, 0.8660254037844387076, 1.000000000000000000, 0.8660254037844387076, 1.000000000000000000, 0.8660254037844387076, 1.000000000000000000, 0.8660254037844387076, 1.000000000000000000, 0.8660254037844387076, 1.000000000000000000, 0.8660254037844387076, 1.000000000000000000, 0.8660254037844387076, 1.000000000000000000, 0.8660254037844387076, 1.000000000000000000, 0.8660254037844387076, 1.000000000000000000, 0.8660254037844387076, 1.000000000000000000, 0.8660254037844387076, 1.000000000000000000, 0.8660254037844387076, 1.000000000000000000, 0.8660254037844387076, 1.000000000000000000, 0.8660254037844387076, 1.000000000000000000, 0.8660254037844387076, 1.000000000000000000, 0.8660254037844387076, 1.000000000000000000, 0.8660254037844387076, 1.000000000000000000, 0.8660254037844387076, 1.000000000000000000),
 ( 1.000000000000000000, 0.8660254037844387076, 1.000000000000000000, 0.8660254037844387076, 1.000000000000000000, 0.8660254037844387076, 1.000000000000000000, 0.8660254037844387076, 1.000000000000000000, 0.8660254037844387076, 1.000000000000000000, 0.8660254037844387076, 1.000000000000000000, 0.8660254037844387076, 1.000000000000000000, 0.8660254037844387076, 1.000000000000000000, 0.8660254037844387076, 1.000000000000000000, 0.8660254037844387076, 1.000000000000000000, 0.8660254037844387076, 1.000000000000000000, 0.8660254037844387076, 1.000000000000000000, 0.8660254037844387076, 1.000000000000000000, 0.8660254037844387076, 1.000000000000000000, 0.8660254037844387076, 1.000000000000000000, 0.8660254037844387076, 1.000000000000000000, 0.8660254037844387076, 1.000000000000000000, 0.8660254037844387076, 1.000000000000000000, 0.8660254037844387076, 1.000000000000000000, 0.8660254037844387076, 1.000000000000000000, 0.8660254037844387076, 1.000000000000000000, 0.8660254037844387076, 1.000000000000000000, 0.8660254037844387076, 1.000000000000000000, 0.8660254037844387076, 1.000000000000000000, 0.8660254037844387076, 1.000000000000000000, 0.8660254037844387076, 1.000000000000000000, 0.8660254037844387076, 1.000000000000000000, 0.8660254037844387076, 1.000000000000000000, 0.8660254037844387076, 1.000000000000000000, 0.8660254037844387076, 1.000000000000000000, 0.8660254037844387076, 1.000000000000000000, 0.8660254037844387076, 1.000000000000000000, 0.8660254037844387076, 1.000000000000000000, 0.8660254037844387076, 1.000000000000000000, 0.8660254037844387076, 1.000000000000000000, 0.8660254037844387076, 1.000000000000000000, 0.8660254037844387076, 1.000000000000000000, 0.8660254037844387076, 1.000000000000000000, 0.8660254037844387076, 1.000000000000000000, 0.8660254037844387076, 1.000000000000000000, 0.8660254037844387076, 1.000000000000000000, 0.8660254037844387076, 1.000000000000000000, 0.8660254037844387076, 1.000000000000000000, 0.8660254037844387076, 1.000000000000000000, 0.8660254037844387076, 1.000000000000000000, 0.8660254037844387076, 1.000000000000000000, 0.8660254037844387076, 1.000000000000000000, 0.8660254037844387076, 1.000000000000000000, 0.8660254037844387076, 1.000000000000000000, 0.8660254037844387076, 1.000000000000000000, 0.8660254037844387076, 1.000000000000000000, 0.8660254037844387076, 1.000000000000000000, 0.8660254037844387076, 1.000000000000000000, 0.8660254037844387076, 1.000000000000000000, 0.8660254037844387076, 1.000000000000000000, 0.8660254037844387076, 1.000000000000000000, 0.8660254037844387076, 1.000000000000000000, 0.8660254037844387076, 1.000000000000000000, 0.8660254037844387076, 1.000000000000000000, 0.8660254037844387076, 1.000000000000000000) ) ) 
 REPRESENTATION_ITEM ( '' )  SURFACE ( )  );
#1064 = ADVANCED_FACE ( 'NONE', ( #24442 ), #12677, .F. ) ;
#1065 = CARTESIAN_POINT ( 'NONE',  ( 3.756430356250002323, -11.16877607737301226, 0.5531249993854806535 ) ) ;
#1066 = CARTESIAN_POINT ( 'NONE',  ( 23.29708626209844269, 17.98469150617961887, 8.999999999999992895 ) ) ;
#1067 = DIRECTION ( 'NONE',  ( -0.000000000000000000, -0.000000000000000000, 1.000000000000000000 ) ) ;
#1068 = EDGE_CURVE ( 'NONE', #1940, #9674, #15367, .T. ) ;
#1069 = CARTESIAN_POINT ( 'NONE',  ( 3.401318489840877923, -30.91344420362549528, -6.500000000000000000 ) ) ;
#1070 = CARTESIAN_POINT ( 'NONE',  ( 2.620986760973688460E-15, -13.61880215351699874, 0.3375000000000008549 ) ) ;
#1071 = DIRECTION ( 'NONE',  ( 0.9048270524660195768, -0.4257792915650726040, 0.000000000000000000 ) ) ;
#1072 = DIRECTION ( 'NONE',  ( -0.7071067811865487940, -0.7071067811865463515, 0.000000000000000000 ) ) ;
#1073 = DIRECTION ( 'NONE',  ( 0.000000000000000000, 0.000000000000000000, 1.000000000000000000 ) ) ;
#1074 = DIRECTION ( 'NONE',  ( 0.000000000000000000, 0.000000000000000000, -1.000000000000000000 ) ) ;
#1075 = CARTESIAN_POINT ( 'NONE',  ( -1.878215178124995832, -5.746835883940462963, 4.453124999385483562 ) ) ;
#1076 = DIRECTION ( 'NONE',  ( 0.000000000000000000, 0.000000000000000000, 1.000000000000000000 ) ) ;
#1077 = CARTESIAN_POINT ( 'NONE',  ( -1.071796769724494558, -25.54240381056766651, 4.999999999999992895 ) ) ;
#1078 = EDGE_LOOP ( 'NONE', ( #22669, #22210, #8277, #12671 ) ) ;
#1079 = ORIENTED_EDGE ( 'NONE', *, *, #19912, .F. ) ;
#1080 = EDGE_LOOP ( 'NONE', ( #4196, #7067, #16369, #11365 ) ) ;
#1081 = DIRECTION ( 'NONE',  ( 0.000000000000000000, 0.000000000000000000, 1.000000000000000000 ) ) ;
#1082 = ORIENTED_EDGE ( 'NONE', *, *, #23440, .T. ) ;
#1083 = AXIS2_PLACEMENT_3D ( 'NONE', #15502, #9739, #17213 ) ;
#1084 = CARTESIAN_POINT ( 'NONE',  ( -2.672651547586948120E-15, -26.04062499938548925, 13.33755215474602984 ) ) ;
#1085 = ORIENTED_EDGE ( 'NONE', *, *, #12027, .F. ) ;
#1086 = DIRECTION ( 'NONE',  ( 1.000000000000000000, 0.000000000000000000, 0.000000000000000000 ) ) ;
#1087 = VERTEX_POINT ( 'NONE', #6518 ) ;
#1088 = CARTESIAN_POINT ( 'NONE',  ( 18.28012134629577190, -25.16042852506097205, 1.000000000000000000 ) ) ;
#1089 = CARTESIAN_POINT ( 'NONE',  ( 4.000000000000003553, 25.00000000000000000, 8.999999999999992895 ) ) ;
#1090 = CARTESIAN_POINT ( 'NONE',  ( -31.03863125411927371, -1.952785157361310198, -6.500000000000000000 ) ) ;
#1091 = DIRECTION ( 'NONE',  ( -0.000000000000000000, -0.000000000000000000, -1.000000000000000000 ) ) ;
#1092 = CARTESIAN_POINT ( 'NONE',  ( 15.67775563255858984, 20.99015038847727155, 8.999999999999992895 ) ) ;
#1093 = ADVANCED_FACE ( 'NONE', ( #14502 ), #10060, .T. ) ;
#1094 = FACE_OUTER_BOUND ( 'NONE', #21501, .T. ) ;
#1095 = CARTESIAN_POINT ( 'NONE',  ( -1.878215178124995832, 29.34062499938548285, 5.746835883940462963 ) ) ;
#1096 = EDGE_CURVE ( 'NONE', #4544, #12039, #7136, .T. ) ;
#1097 = CARTESIAN_POINT ( 'NONE',  ( 21.17576591853880075, 15.86337116261998048, 6.831223922626973533 ) ) ;
#1098 = CARTESIAN_POINT ( 'NONE',  ( 3.469446951953614189E-15, 30.00000000000000355, 8.999999999999992895 ) ) ;
#1099 = ORIENTED_EDGE ( 'NONE', *, *, #1162, .T. ) ;
#1100 = CARTESIAN_POINT ( 'NONE',  ( -3.999999999999996447, 27.83124999877097139, 6.690598923241487306 ) ) ;
#1101 = CARTESIAN_POINT ( 'NONE',  ( 1.878215178124998497, -27.69062499938548427, 12.25316411605951927 ) ) ;
#1102 = ADVANCED_FACE ( 'NONE', ( #24794 ), #25186, .F. ) ;
#1103 = CARTESIAN_POINT ( 'NONE',  ( 25.99307600111999150, -0.5999999999999998668, 20.00001200000000168 ) ) ;
#1104 = CARTESIAN_POINT ( 'NONE',  ( 3.756430356250003655, 27.50312499938548427, 8.999999999999992895 ) ) ;
#1105 = CARTESIAN_POINT ( 'NONE',  ( 0.5788183228083377818, 29.99578766836522092, 12.96878440844335678 ) ) ;
#1107 = ORIENTED_EDGE ( 'NONE', *, *, #2812, .T. ) ;
#1106 = CARTESIAN_POINT ( 'NONE',  ( 1.878215178125001605, 28.77812499938549351, 12.25316411605952283 ) ) ;
#1108 = EDGE_LOOP ( 'NONE', ( #16463, #25740, #25010, #7826 ) ) ;
#1109 = LINE ( 'NONE', #15243, #13742 ) ;
#1110 = CARTESIAN_POINT ( 'NONE',  ( 1.071796769724492338, 26.20134618820330275, 12.99999999999999467 ) ) ;
#1111 = VERTEX_POINT ( 'NONE', #20862 ) ;
#1112 = CARTESIAN_POINT ( 'NONE',  ( -3.735045420075836212E-15, -29.41562499938548569, 4.662447845253954171 ) ) ;
#1113 = CARTESIAN_POINT ( 'NONE',  ( 4.000000000000003553, 25.93750000000000000, 6.690598923241489970 ) ) ;
#1114 = CARTESIAN_POINT ( 'NONE',  ( -1.878215178124996498, 25.74062499938548854, 5.746835883940462963 ) ) ;
#1115 = CARTESIAN_POINT ( 'NONE',  ( 20.94803839265150458, 18.11961126790524901, 12.46410161513774817 ) ) ;
#1116 = CARTESIAN_POINT ( 'NONE',  ( 3.756430356250003211, 28.29062499938548569, 8.999999999999992895 ) ) ;
#1117 = DIRECTION ( 'NONE',  ( 0.9685831611286301879, -0.2486898871648584586, 0.000000000000000000 ) ) ;
#1118 =( NAMED_UNIT ( * ) PLANE_ANGLE_UNIT ( ) SI_UNIT ( $, .RADIAN. ) );
#1119 = CARTESIAN_POINT ( 'NONE',  ( -1.999999999999995781, 26.95000000000000284, 5.535898384862237620 ) ) ;
#1120 = SHAPE_REPRESENTATION ( 'glass', ( #21036 ), #9344 ) ;
#1121 = LINE ( 'NONE', #3476, #23861 ) ;
#1122 = EDGE_CURVE ( 'NONE', #18910, #5387, #12620, .T. ) ;
#1123 = CARTESIAN_POINT ( 'NONE',  ( -1.878215178124995832, 26.64062499938548711, 5.746835883940462963 ) ) ;
#1124 = CARTESIAN_POINT ( 'NONE',  ( -4.000000000000002665, -29.73213749463701205, 8.735714247490120599 ) ) ;
#1125 = CARTESIAN_POINT ( 'NONE',  ( 17.85210898470722896, 23.16450374062589646, 11.16877607737301226 ) ) ;
#1126 = CARTESIAN_POINT ( 'NONE',  ( 22.49925389301043666, 19.67082676826417398, 12.46410161513774817 ) ) ;
#1127 = CARTESIAN_POINT ( 'NONE',  ( 17.26224429571663066, 22.91909854520893930, 11.30940107675849404 ) ) ;
#1128 = CARTESIAN_POINT ( 'NONE',  ( 3.756430356250004099, 27.87812499938548427, 6.831223922626973533 ) ) ;
#1130 = EDGE_CURVE ( 'NONE', #17660, #23467, #24227, .T. ) ;
#1129 = DIRECTION ( 'NONE',  ( -0.000000000000000000, 1.000000000000000000, -0.000000000000000000 ) ) ;
#1131 = CARTESIAN_POINT ( 'NONE',  ( 20.43103032403801578, 17.77483294607857189, 5.746835883940462963 ) ) ;
#1132 = CARTESIAN_POINT ( 'NONE',  ( 3.137519842735244810E-15, -26.85624999877096641, 4.999999999999991118 ) ) ;
#1133 = EDGE_CURVE ( 'NONE', #25152, #672, #3440, .T. ) ;
#1134 = ORIENTED_EDGE ( 'NONE', *, *, #19392, .F. ) ;
#1135 = CARTESIAN_POINT ( 'NONE',  ( -3.999999999999995559, 28.78750000000000142, 6.690598923241487306 ) ) ;
#1136 = CARTESIAN_POINT ( 'NONE',  ( 2.000000000000003997, 27.26874999877097139, 5.535898384862238508 ) ) ;
#1137 = CARTESIAN_POINT ( 'NONE',  ( 1.878215178124998497, -29.49062499938548498, 12.25316411605951927 ) ) ;
#1139 = VERTEX_POINT ( 'NONE', #19031 ) ;
#1138 = CARTESIAN_POINT ( 'NONE',  ( 5.577813053751546416E-15, 25.33750000000000213, 12.99999999999999289 ) ) ;
#1140 = CARTESIAN_POINT ( 'NONE',  ( 1.878215178125000939, 26.07812499938548356, 12.25316411605952283 ) ) ;
#1141 = VERTEX_POINT ( 'NONE', #3084 ) ;
#1142 = CARTESIAN_POINT ( 'NONE',  ( -3.756430356250003655, -27.39062499938548356, 8.999999999999992895 ) ) ;
#1143 = VERTEX_POINT ( 'NONE', #18649 ) ;
#1144 = EDGE_CURVE ( 'NONE', #20048, #24513, #24920, .T. ) ;
#1145 = ORIENTED_EDGE ( 'NONE', *, *, #19132, .F. ) ;
#1146 = CARTESIAN_POINT ( 'NONE',  ( 18.29814930579269827, 23.77352349748025517, 7.961019890438434388 ) ) ;
#1147 = CARTESIAN_POINT ( 'NONE',  ( 3.756430356250006319, 27.09062499938548285, 6.831223922626973533 ) ) ;
#1148 = CARTESIAN_POINT ( 'NONE',  ( -3.756430356249997438, -11.16877607737301048, 0.8531249993854844726 ) ) ;
#1149 = DIRECTION ( 'NONE',  ( 1.000000000000000000, 0.000000000000000000, 0.000000000000000000 ) ) ;
#1150 = ADVANCED_FACE ( 'NONE', ( #17075 ), #10655, .F. ) ;
#1151 = DIRECTION ( 'NONE',  ( 0.000000000000000000, 1.000000000000000000, 0.000000000000000000 ) ) ;
#1152 = CARTESIAN_POINT ( 'NONE',  ( 4.648177544792955347E-16, 26.68750000000000711, 12.99999999999999289 ) ) ;
#1153 = CYLINDRICAL_SURFACE ( 'NONE', #17186, 4.000000000000000000 ) ;
#1154 = CARTESIAN_POINT ( 'NONE',  ( 2.672651547586948120E-15, 28.62812499938548783, 13.33755215474603162 ) ) ;
#1155 = LINE ( 'NONE', #20782, #4194 ) ;
#1156 = CARTESIAN_POINT ( 'NONE',  ( -3.834746474454188013E-15, -25.56250000000000000, 4.999999999999992006 ) ) ;
#1157 = CYLINDRICAL_SURFACE ( 'NONE', #15557, 0.5000000000000004441 ) ;
#1158 = DIRECTION ( 'NONE',  ( 0.8443279255020205154, 0.5358267949789882190, 0.000000000000000000 ) ) ;
#1159 = CARTESIAN_POINT ( 'NONE',  ( -2.672651547586948120E-15, -29.64062499938548356, 13.33755215474602984 ) ) ;
#1160 = CARTESIAN_POINT ( 'NONE',  ( -3.756430356249997882, 26.41562499938548569, 11.16877607737301226 ) ) ;
#1162 = EDGE_CURVE ( 'NONE', #7703, #23505, #732, .T. ) ;
#1161 = CARTESIAN_POINT ( 'NONE',  ( 4.000000000000003553, 27.68124999877096926, 6.690598923241489970 ) ) ;
#1163 = CARTESIAN_POINT ( 'NONE',  ( 8.831537335106614961E-15, 27.13750000000000284, 12.99999999999999112 ) ) ;
#1164 = CARTESIAN_POINT ( 'NONE',  ( 3.595408253811773758, -29.78394301743083261, 10.77252090037689136 ) ) ;
#1165 = ORIENTED_EDGE ( 'NONE', *, *, #15711, .T. ) ;
#1166 = DIRECTION ( 'NONE',  ( 0.000000000000000000, 0.000000000000000000, 1.000000000000000000 ) ) ;
#1168 = VERTEX_POINT ( 'NONE', #8701 ) ;
#1167 = DIRECTION ( 'NONE',  ( 0.000000000000000000, 0.000000000000000000, 1.000000000000000000 ) ) ;
#1169 = EDGE_CURVE ( 'NONE', #4288, #22996, #9088, .T. ) ;
#1170 = ORIENTED_EDGE ( 'NONE', *, *, #23564, .T. ) ;
#1171 = AXIS2_PLACEMENT_3D ( 'NONE', #304, #18486, #14429 ) ;
#1172 = EDGE_LOOP ( 'NONE', ( #1838, #14310, #24792, #24076 ) ) ;
#1173 = VERTEX_POINT ( 'NONE', #5181 ) ;
#1174 = EDGE_CURVE ( 'NONE', #11752, #12276, #996, .T. ) ;
#1175 = VERTEX_POINT ( 'NONE', #16952 ) ;
#1176 = LINE ( 'NONE', #19354, #17236 ) ;
#1178 = EDGE_CURVE ( 'NONE', #12169, #3229, #4908, .T. ) ;
#1177 = DIRECTION ( 'NONE',  ( -0.000000000000000000, -1.000000000000000000, -0.000000000000000000 ) ) ;
#1179 = AXIS2_PLACEMENT_3D ( 'NONE', #659, #8628, #6530 ) ;
#1180 = CARTESIAN_POINT ( 'NONE',  ( -30.00000000000000355, 0.000000000000000000, 20.00000000000000000 ) ) ;
#1181 = CARTESIAN_POINT ( 'NONE',  ( 1.878215178125004048, -5.746835883940462963, 4.378124999385484273 ) ) ;
#1182 = CARTESIAN_POINT ( 'NONE',  ( 2.000000000000003997, -5.535898384862238508, 1.818749998770966769 ) ) ;
#1183 = CARTESIAN_POINT ( 'NONE',  ( 19.92494326818769323, 19.92494326818762218, 13.33755215474602984 ) ) ;
#1184 = CARTESIAN_POINT ( 'NONE',  ( 3.756430356250004099, 26.19062499938548783, 6.831223922626973533 ) ) ;
#1185 = CARTESIAN_POINT ( 'NONE',  ( -4.000000000000001776, -26.70624999877097139, 11.30940107675849760 ) ) ;
#1186 = VECTOR ( 'NONE', #9407, 1000.000000000000000 ) ;
#1187 = CARTESIAN_POINT ( 'NONE',  ( 0.000000000000000000, 29.78124999877097423, 12.99999999999999289 ) ) ;
#1188 = CARTESIAN_POINT ( 'NONE',  ( 3.756430356250002323, -11.16877607737301226, 4.603124999385482141 ) ) ;
#1189 = CIRCLE ( 'NONE', #25014, 0.5000000000000002220 ) ;
#1190 = DIRECTION ( 'NONE',  ( 0.000000000000000000, 0.000000000000000000, -1.000000000000000000 ) ) ;
#1191 = CARTESIAN_POINT ( 'NONE',  ( 3.878215178125005380, 29.57031249969274356, 8.999999999999992895 ) ) ;
#1192 = CARTESIAN_POINT ( 'NONE',  ( 17.48763458135079318, 23.14448883084309827, 6.690598923241487306 ) ) ;
#1193 = CARTESIAN_POINT ( 'NONE',  ( -3.752267015613588906E-15, -25.50624999877097565, 4.381197846482986158 ) ) ;
#1194 = CARTESIAN_POINT ( 'NONE',  ( 3.756430356250003211, -6.831223922626973533, 3.890624999385483562 ) ) ;
#1195 = AXIS2_PLACEMENT_3D ( 'NONE', #2275, #8944, #823 ) ;
#1196 = DIRECTION ( 'NONE',  ( 1.000000000000000000, 0.000000000000000000, 0.000000000000000000 ) ) ;
#1197 = VECTOR ( 'NONE', #3668, 1000.000000000000000 ) ;
#1198 = DIRECTION ( 'NONE',  ( 1.000000000000000000, 0.000000000000000000, 0.000000000000000000 ) ) ;
#1199 = ORIENTED_EDGE ( 'NONE', *, *, #5496, .T. ) ;
#1200 = DIRECTION ( 'NONE',  ( -0.000000000000000000, -0.000000000000000000, 1.000000000000000000 ) ) ;
#1201 = ORIENTED_EDGE ( 'NONE', *, *, #18891, .T. ) ;
#1202 = ORIENTED_EDGE ( 'NONE', *, *, #12840, .F. ) ;
#1203 = CARTESIAN_POINT ( 'NONE',  ( -30.63887302793240508, 5.335677986745117174, -6.500000000000000000 ) ) ;
#1204 = ORIENTED_EDGE ( 'NONE', *, *, #21065, .F. ) ;
#1205 = CARTESIAN_POINT ( 'NONE',  ( -3.735045420075836212E-15, -26.71562499938548640, 4.662447845253954171 ) ) ;
#1206 = EDGE_CURVE ( 'NONE', #10563, #17279, #13544, .T. ) ;
#1207 = EDGE_LOOP ( 'NONE', ( #8391, #20008, #11792, #25836 ) ) ;
#1208 = DIRECTION ( 'NONE',  ( 0.000000000000000000, 1.000000000000000000, 0.000000000000000000 ) ) ;
#1209 =( BOUNDED_CURVE ( )  B_SPLINE_CURVE ( 2, ( #19108, #17166, #3281, #7221, #15205, #23173, #11254 ),
 .UNSPECIFIED., .F., .F. ) 
 B_SPLINE_CURVE_WITH_KNOTS ( ( 3, 2, 2, 3 ),
 ( 0.000000000000000000, 0.01666666666666663521, 0.03333333333333327042, 0.04999999999999990563 ),
 .UNSPECIFIED. ) 
 CURVE ( )  GEOMETRIC_REPRESENTATION_ITEM ( )  RATIONAL_B_SPLINE_CURVE ( ( 1.000000000000000000, 0.8660254037844387076, 1.000000000000000000, 0.8660254037844387076, 1.000000000000000000, 0.8660254037844394848, 0.9999999999999992228 ) ) 
 REPRESENTATION_ITEM ( '' )  );
#1210 = ADVANCED_FACE ( 'NONE', ( #3711 ), #1900, .F. ) ;
#1211 = VECTOR ( 'NONE', #750, 1000.000000000000000 ) ;
#1212 = ORIENTED_EDGE ( 'NONE', *, *, #17247, .T. ) ;
#1213 = FACE_OUTER_BOUND ( 'NONE', #5482, .T. ) ;
#1214 = CARTESIAN_POINT ( 'NONE',  ( -1.878215178124998497, 28.59062499938548285, 12.25316411605951927 ) ) ;
#1215 = EDGE_CURVE ( 'NONE', #17650, #15811, #15635, .T. ) ;
#1216 = CARTESIAN_POINT ( 'NONE',  ( 1.071796769724487230, -27.38259618943233420, 4.999999999999992006 ) ) ;
#1217 = AXIS2_PLACEMENT_3D ( 'NONE', #13567, #5586, #21034 ) ;
#1218 = VECTOR ( 'NONE', #19343, 1000.000000000000000 ) ;
#1219 = CARTESIAN_POINT ( 'NONE',  ( -3.999999999999996447, 26.57500000000000284, 8.999999999999992895 ) ) ;
#1220 = DIRECTION ( 'NONE',  ( 0.000000000000000000, -0.000000000000000000, 1.000000000000000000 ) ) ;
#1221 = CARTESIAN_POINT ( 'NONE',  ( 16.31415173562648491, 21.62654649154516306, 8.999999999999992895 ) ) ;
#1222 = DIRECTION ( 'NONE',  ( 0.000000000000000000, 0.000000000000000000, 1.000000000000000000 ) ) ;
#1223 = CARTESIAN_POINT ( 'NONE',  ( 1.878215178125000939, 29.56562499938548427, 12.25316411605952283 ) ) ;
#1224 = CARTESIAN_POINT ( 'NONE',  ( 21.44093096148375466, 16.12853620556493794, 11.16877607737301403 ) ) ;
#1225 = FACE_OUTER_BOUND ( 'NONE', #6945, .T. ) ;
#1226 = AXIS2_PLACEMENT_3D ( 'NONE', #21445, #15428, #23533 ) ;
#1227 = ORIENTED_EDGE ( 'NONE', *, *, #15608, .T. ) ;
#1228 = VERTEX_POINT ( 'NONE', #17343 ) ;
#1229 = CARTESIAN_POINT ( 'NONE',  ( 2.000000000000000000, 28.91874999877097707, 12.46410161513774817 ) ) ;
#1230 = AXIS2_PLACEMENT_3D ( 'NONE', #16542, #15612, #7365 ) ;
#1231 = DIRECTION ( 'NONE',  ( 1.000000000000000000, 0.000000000000000000, 0.000000000000000000 ) ) ;
#1232 = AXIS2_PLACEMENT_3D ( 'NONE', #10906, #22821, #1231 ) ;
#1233 = CARTESIAN_POINT ( 'NONE',  ( -3.756430356249996994, 27.27812499938548640, 8.999999999999992895 ) ) ;
#1234 = DIRECTION ( 'NONE',  ( 0.000000000000000000, 1.000000000000000000, 0.000000000000000000 ) ) ;
#1235 = ORIENTED_EDGE ( 'NONE', *, *, #22619, .T. ) ;
#1236 = EDGE_LOOP ( 'NONE', ( #16558, #5111, #1058, #21230 ) ) ;
#1237 = CARTESIAN_POINT ( 'NONE',  ( -3.397863563850083146, -30.85476721088024021, 1.000000000000000000 ) ) ;
#1238 = ADVANCED_FACE ( 'NONE', ( #9863 ), #7774, .T. ) ;
#1239 = CARTESIAN_POINT ( 'NONE',  ( 0.000000000000000000, 0.000000000000000000, 1.000000000000000000 ) ) ;
#1240 = AXIS2_PLACEMENT_3D ( 'NONE', #4577, #12555, #8637 ) ;
#1241 = ORIENTED_EDGE ( 'NONE', *, *, #14257, .F. ) ;
#1242 = CARTESIAN_POINT ( 'NONE',  ( 3.756430356249996105, -29.04062499938548569, 6.831223922626973533 ) ) ;
#1243 = CARTESIAN_POINT ( 'NONE',  ( -27.25313774936397948, 14.98253926456367502, -6.500000000000000000 ) ) ;
#1244 = CARTESIAN_POINT ( 'NONE',  ( -1.878215178124999829, 26.34062499938548996, 12.25316411605951927 ) ) ;
#1245 = AXIS2_PLACEMENT_3D ( 'NONE', #6493, #22719, #12504 ) ;
#1246 = VECTOR ( 'NONE', #15657, 1000.000000000000000 ) ;
#1247 = CARTESIAN_POINT ( 'NONE',  ( 21.05410440982949183, 18.22567728508322205, 5.535898384862238508 ) ) ;
#1248 = CARTESIAN_POINT ( 'NONE',  ( -1.999999999999998224, 25.75000000000000711, 12.46410161513774639 ) ) ;
#1249 = AXIS2_PLACEMENT_3D ( 'NONE', #11596, #19570, #3891 ) ;
#1250 = EDGE_CURVE ( 'NONE', #6185, #21954, #25154, .T. ) ;
#1251 = DIRECTION ( 'NONE',  ( -0.000000000000000000, 0.000000000000000000, 1.000000000000000000 ) ) ;
#1252 = PRODUCT_CONTEXT ( 'NONE', #12277, 'mechanical' ) ;
#1253 = CARTESIAN_POINT ( 'NONE',  ( -9.610428525061097460, -29.57785765677920509, 1.000000000000000000 ) ) ;
#1254 = DIRECTION ( 'NONE',  ( 1.000000000000000000, 0.000000000000000000, 0.000000000000000000 ) ) ;
#1255 = CARTESIAN_POINT ( 'NONE',  ( 1.878215178125000939, 26.86562499938548498, 12.25316411605952283 ) ) ;
#1256 = CIRCLE ( 'NONE', #21720, 0.5000000000000002220 ) ;
#1257 = CARTESIAN_POINT ( 'NONE',  ( -2.444316569969958497, -29.90105888194226580, 5.822820249163556561 ) ) ;
#1258 = CARTESIAN_POINT ( 'NONE',  ( 17.53391093317328142, 22.84630568909195958, 11.16877607737301226 ) ) ;
#1259 = CARTESIAN_POINT ( 'NONE',  ( 19.55598568231966539, 16.89978830436022150, 5.746835883940462963 ) ) ;
#1260 = CARTESIAN_POINT ( 'NONE',  ( 31.06601413805602263, -1.453535542772716793, -2.750000000000000000 ) ) ;
#1261 = CARTESIAN_POINT ( 'NONE',  ( 3.756430356250002323, 27.80312499938548143, 11.16877607737301226 ) ) ;
#1262 = CIRCLE ( 'NONE', #5428, 0.5000000000000003331 ) ;
#1263 = CARTESIAN_POINT ( 'NONE',  ( -3.469446951953614189E-15, -25.00000000000000000, 8.999999999999992895 ) ) ;
#1264 = AXIS2_PLACEMENT_3D ( 'NONE', #25584, #5697, #1523 ) ;
#1265 = CARTESIAN_POINT ( 'NONE',  ( 17.18919637734483885, 22.50159113326351346, 8.999999999999992895 ) ) ;
#1266 = CARTESIAN_POINT ( 'NONE',  ( 21.51241069055853927, 19.99666116270642036, 12.99999999999999467 ) ) ;
#1267 = ORIENTED_EDGE ( 'NONE', *, *, #17537, .T. ) ;
#1268 = CARTESIAN_POINT ( 'NONE',  ( 21.46069080901174786, 15.80383655951930066, 8.999999999999992895 ) ) ;
#1269 = CARTESIAN_POINT ( 'NONE',  ( 3.735045420075836212E-15, 26.26562499938548356, 4.662447845253954171 ) ) ;
#1270 = CARTESIAN_POINT ( 'NONE',  ( -3.756430356250003655, -29.19062499938548072, 8.999999999999992895 ) ) ;
#1272 = ORIENTED_EDGE ( 'NONE', *, *, #18531, .T. ) ;
#1271 = DIRECTION ( 'NONE',  ( 0.000000000000000000, 0.000000000000000000, 1.000000000000000000 ) ) ;
#1273 = CARTESIAN_POINT ( 'NONE',  ( -3.756430356249997438, 25.96562499938548640, 11.16877607737301048 ) ) ;
#1274 = VECTOR ( 'NONE', #23416, 1000.000000000000000 ) ;
#1275 = ORIENTED_EDGE ( 'NONE', *, *, #7993, .T. ) ;
#1276 = CARTESIAN_POINT ( 'NONE',  ( -3.756430356250002323, -28.25312499938548427, 11.16877607737301226 ) ) ;
#1277 = VERTEX_POINT ( 'NONE', #21768 ) ;
#1278 = EDGE_LOOP ( 'NONE', ( #4589, #25272, #5489, #14857 ) ) ;
#1279 = DIRECTION ( 'NONE',  ( 0.000000000000000000, 1.000000000000000000, 0.000000000000000000 ) ) ;
#1280 = CARTESIAN_POINT ( 'NONE',  ( -3.756430356249996105, 27.76562499938549422, 11.16877607737301226 ) ) ;
#1281 = CIRCLE ( 'NONE', #10881, 0.5000000000000002220 ) ;
#1282 = ADVANCED_FACE ( 'NONE', ( #25814 ), #7386, .T. ) ;
#1283 = CARTESIAN_POINT ( 'NONE',  ( -3.756430356249996105, -6.831223922626973533, 0.7781249993854825187 ) ) ;
#1284 = VECTOR ( 'NONE', #21794, 1000.000000000000000 ) ;
#1285 = AXIS2_PLACEMENT_3D ( 'NONE', #1608, #11806, #20026 ) ;
#1286 = DIRECTION ( 'NONE',  ( 0.000000000000000000, 0.000000000000000000, 1.000000000000000000 ) ) ;
#1287 = AXIS2_PLACEMENT_3D ( 'NONE', #614, #20207, #6093 ) ;
#1288 = CARTESIAN_POINT ( 'NONE',  ( -4.000000000000003553, -27.25000000000000000, 8.999999999999992895 ) ) ;
#1289 = AXIS2_PLACEMENT_3D ( 'NONE', #7040, #4829, #16993 ) ;
#1290 = CARTESIAN_POINT ( 'NONE',  ( 2.000000000000003553, 29.12500000000000355, 5.535898384862238508 ) ) ;
#1291 = LINE ( 'NONE', #5217, #20952 ) ;
#1292 = UNCERTAINTY_MEASURE_WITH_UNIT (LENGTH_MEASURE( 1.000000000000000082E-05 ), #12896, 'distance_accuracy_value', 'NONE');
#1293 = FACE_OUTER_BOUND ( 'NONE', #4147, .T. ) ;
#1294 = FACE_OUTER_BOUND ( 'NONE', #19245, .T. ) ;
#1295 = CARTESIAN_POINT ( 'NONE',  ( 9.610428525060671134, -29.57785765677934009, -6.500000000000000000 ) ) ;
#1296 = DIRECTION ( 'NONE',  ( 0.7071067811865487940, 0.7071067811865463515, -0.000000000000000000 ) ) ;
#1297 = LINE ( 'NONE', #23257, #6343 ) ;
#1298 = CARTESIAN_POINT ( 'NONE',  ( 3.756430356249997882, -29.11562499938548143, 11.16877607737301226 ) ) ;
#1299 = CARTESIAN_POINT ( 'NONE',  ( 2.672651547586948120E-15, 26.04062499938548925, 13.33755215474602984 ) ) ;
#1300 = CARTESIAN_POINT ( 'NONE',  ( 2.000000000000003997, 27.71874999877097068, 5.535898384862238508 ) ) ;
#1301 = VECTOR ( 'NONE', #19260, 1000.000000000000000 ) ;
#1302 = CARTESIAN_POINT ( 'NONE',  ( -27.10000000000000497, -0.5999999999999998668, 19.59999999999999787 ) ) ;
#1303 = ADVANCED_BREP_SHAPE_REPRESENTATION ( '', ( #5435, #21036 ), #582 ) ;
#1304 = CARTESIAN_POINT ( 'NONE',  ( -29.41953157733080104, 10.08469938919530584, -2.750000000000000000 ) ) ;
#1305 = VERTEX_POINT ( 'NONE', #5426 ) ;
#1306 = CARTESIAN_POINT ( 'NONE',  ( 1.071796769724488563, -27.06115380933863435, 12.99999999999999289 ) ) ;
#1307 = FACE_OUTER_BOUND ( 'NONE', #12729, .T. ) ;
#1309 = VERTEX_POINT ( 'NONE', #5680 ) ;
#1308 = CARTESIAN_POINT ( 'NONE',  ( 21.21320343559646915, 21.21320343559638744, 12.99999999999999289 ) ) ;
#1310 = AXIS2_PLACEMENT_3D ( 'NONE', #12384, #20350, #10407 ) ;
#1311 = EDGE_LOOP ( 'NONE', ( #346, #6595, #13086, #8643 ) ) ;
#1312 = ORIENTED_EDGE ( 'NONE', *, *, #25575, .F. ) ;
#1313 = VERTEX_POINT ( 'NONE', #11561 ) ;
#1314 = EDGE_CURVE ( 'NONE', #16500, #21799, #19529, .T. ) ;
#1315 = VERTEX_POINT ( 'NONE', #13659 ) ;
#1316 = DIRECTION ( 'NONE',  ( 0.000000000000000000, 0.000000000000000000, -1.000000000000000000 ) ) ;
#1318 = CYLINDRICAL_SURFACE ( 'NONE', #6505, 4.000000000000000000 ) ;
#1317 = CIRCLE ( 'NONE', #12586, 0.4999999999999993894 ) ;
#1319 = EDGE_CURVE ( 'NONE', #14821, #23630, #19800, .T. ) ;
#1320 = FACE_OUTER_BOUND ( 'NONE', #10555, .T. ) ;
#1321 = EDGE_CURVE ( 'NONE', #10871, #23470, #3412, .T. ) ;
#1322 = VECTOR ( 'NONE', #7540, 1000.000000000000000 ) ;
#1323 = CARTESIAN_POINT ( 'NONE',  ( 1.878215178125004048, -5.746835883940462963, 1.565624999385482274 ) ) ;
#1324 = CARTESIAN_POINT ( 'NONE',  ( -1.999999999999995781, -5.535898384862237620, 1.443749998770966325 ) ) ;
#1325 = PRODUCT_DEFINITION_SHAPE ( 'NONE', 'NONE',  #25883 ) ;
#1326 = ADVANCED_FACE ( 'NONE', ( #13414 ), #3053, .T. ) ;
#1327 = AXIS2_PLACEMENT_3D ( 'NONE', #16855, #1020, #18555 ) ;
#1328 = CARTESIAN_POINT ( 'NONE',  ( -3.756430356249997882, 25.51562499938548356, 11.16877607737301226 ) ) ;
#1329 = CIRCLE ( 'NONE', #21778, 0.5000000000000003331 ) ;
#1330 = FACE_OUTER_BOUND ( 'NONE', #4234, .T. ) ;
#1331 = DIRECTION ( 'NONE',  ( 0.000000000000000000, 1.000000000000000000, 0.000000000000000000 ) ) ;
#1332 = CARTESIAN_POINT ( 'NONE',  ( -1.878215178124995832, -5.746835883940462963, 2.990624999385481431 ) ) ;
#1333 = VECTOR ( 'NONE', #12312, 1000.000000000000000 ) ;
#1334 = LINE ( 'NONE', #11391, #10437 ) ;
#1336 = ADVANCED_FACE ( 'NONE', ( #1988 ), #4458, .F. ) ;
#1335 = DIRECTION ( 'NONE',  ( -0.000000000000000000, -0.000000000000000000, 1.000000000000000000 ) ) ;
#1337 = CARTESIAN_POINT ( 'NONE',  ( 19.51936408540558077, 21.03511361325754692, 4.999999999999992006 ) ) ;
#1338 = CARTESIAN_POINT ( 'NONE',  ( 3.999999999999996447, -26.06874999877096855, 8.999999999999992895 ) ) ;
#1339 = AXIS2_PLACEMENT_3D ( 'NONE', #7048, #20294, #10224 ) ;
#1340 = CARTESIAN_POINT ( 'NONE',  ( 3.756430356250003211, -6.831223922626973533, 3.440624999385483829 ) ) ;
#1341 = CARTESIAN_POINT ( 'NONE',  ( 5.577813053751546416E-15, 25.33750000000000924, 12.99999999999999289 ) ) ;
#1342 = DIRECTION ( 'NONE',  ( 0.000000000000000000, 0.000000000000000000, 1.000000000000000000 ) ) ;
#1343 = VERTEX_POINT ( 'NONE', #15994 ) ;
#1344 = CARTESIAN_POINT ( 'NONE',  ( 16.66421332384682685, 26.25859848311265310, -6.500000000000000000 ) ) ;
#1345 = VERTEX_POINT ( 'NONE', #15853 ) ;
#1346 = ORIENTED_EDGE ( 'NONE', *, *, #22021, .T. ) ;
#1347 = FACE_OUTER_BOUND ( 'NONE', #5617, .T. ) ;
#1348 = VERTEX_POINT ( 'NONE', #20279 ) ;
#1349 = CARTESIAN_POINT ( 'NONE',  ( -1.878215178125004048, -28.92812499938548854, 5.746835883940462963 ) ) ;
#1350 = ORIENTED_EDGE ( 'NONE', *, *, #3402, .F. ) ;
#1351 = FACE_OUTER_BOUND ( 'NONE', #3967, .T. ) ;
#1352 = VECTOR ( 'NONE', #18435, 1000.000000000000000 ) ;
#1353 = VECTOR ( 'NONE', #17499, 1000.000000000000000 ) ;
#1354 = ORIENTED_EDGE ( 'NONE', *, *, #17162, .T. ) ;
#1355 = AXIS2_PLACEMENT_3D ( 'NONE', #6744, #12886, #22834 ) ;
#1356 = CARTESIAN_POINT ( 'NONE',  ( -3.999999999999997335, 27.96250000000000213, 11.30940107675849404 ) ) ;
#1357 = DIRECTION ( 'NONE',  ( 1.000000000000000000, 0.000000000000000000, 0.000000000000000000 ) ) ;
#1358 = VECTOR ( 'NONE', #8290, 1000.000000000000114 ) ;
#1359 = CARTESIAN_POINT ( 'NONE',  ( -3.137519842735244810E-15, 26.46249999999999858, 4.999999999999991118 ) ) ;
#1360 = PRODUCT_DEFINITION ( 'UNKNOWN', '', #16061, #7043 ) ;
#1361 = CARTESIAN_POINT ( 'NONE',  ( -22.17092431280609333, -21.28941499438201745, 1.000000000000000000 ) ) ;
#1362 = CARTESIAN_POINT ( 'NONE',  ( 20.85756786700484966, 15.54517311108603472, 6.831223922626973533 ) ) ;
#1363 = CARTESIAN_POINT ( 'NONE',  ( 3.469446951953614189E-15, 35.50000000000000711, 8.999999999999992895 ) ) ;
#1364 = AXIS2_PLACEMENT_3D ( 'NONE', #21070, #13486, #3400 ) ;
#1365 = EDGE_CURVE ( 'NONE', #21478, #1940, #2376, .T. ) ;
#1366 = CARTESIAN_POINT ( 'NONE',  ( 2.000000000000003997, 25.52500000000000213, 5.535898384862238508 ) ) ;
#1367 = EDGE_CURVE ( 'NONE', #19382, #4582, #423, .T. ) ;
#1368 = CARTESIAN_POINT ( 'NONE',  ( 19.20899765223631661, 19.20899765223624200, 4.662447845253954171 ) ) ;
#1369 = DIRECTION ( 'NONE',  ( 1.000000000000000000, 0.000000000000000000, 0.000000000000000000 ) ) ;
#1370 = ORIENTED_EDGE ( 'NONE', *, *, #24143, .T. ) ;
#1371 = ORIENTED_EDGE ( 'NONE', *, *, #18568, .F. ) ;
#1372 = CARTESIAN_POINT ( 'NONE',  ( -3.999999999999994671, 28.73124999877096997, 6.690598923241487306 ) ) ;
#1373 = CARTESIAN_POINT ( 'NONE',  ( 3.756430356249996994, -28.96562499938548285, 8.999999999999992895 ) ) ;
#1374 = ORIENTED_EDGE ( 'NONE', *, *, #24355, .F. ) ;
#1375 = DIRECTION ( 'NONE',  ( 0.000000000000000000, 0.000000000000000000, 1.000000000000000000 ) ) ;
#1376 = CARTESIAN_POINT ( 'NONE',  ( 1.878215178125000939, 27.42812499938548498, 12.25316411605952283 ) ) ;
#1377 = DIRECTION ( 'NONE',  ( 0.000000000000000000, 1.000000000000000000, 0.000000000000000000 ) ) ;
#1378 = ORIENTED_EDGE ( 'NONE', *, *, #11699, .F. ) ;
#1379 = ORIENTED_EDGE ( 'NONE', *, *, #17227, .F. ) ;
#1380 = DIRECTION ( 'NONE',  ( 0.000000000000000000, 0.000000000000000000, 1.000000000000000000 ) ) ;
#1381 = PRESENTATION_LAYER_ASSIGNMENT (  '', '', ( #20584 ) ) ;
#1382 = CARTESIAN_POINT ( 'NONE',  ( 3.469446951953614189E-15, 39.50000000000000000, 8.999999999999992895 ) ) ;
#1383 = ORIENTED_EDGE ( 'NONE', *, *, #9460, .T. ) ;
#1384 = CARTESIAN_POINT ( 'NONE',  ( -1.878215178125000939, -28.77812499938548640, 12.25316411605952283 ) ) ;
#1385 = CARTESIAN_POINT ( 'NONE',  ( 0.000000000000000000, 0.000000000000000000, 17.00000000000000000 ) ) ;
#1386 = CARTESIAN_POINT ( 'NONE',  ( 0.000000000000000000, 27.72812499938548569, 13.33755215474603162 ) ) ;
#1387 = VECTOR ( 'NONE', #11364, 1000.000000000000000 ) ;
#1388 = DIRECTION ( 'NONE',  ( -0.000000000000000000, -0.000000000000000000, 1.000000000000000000 ) ) ;
#1389 = CARTESIAN_POINT ( 'NONE',  ( 1.878215178125003382, 28.36562499938548498, 5.746835883940462963 ) ) ;
#1390 = CIRCLE ( 'NONE', #16014, 31.10000000000000142 ) ;
#1391 = EDGE_CURVE ( 'NONE', #132, #18031, #4665, .T. ) ;
#1392 = PRODUCT_CONTEXT ( 'NONE', #10427, 'mechanical' ) ;
#1393 = CARTESIAN_POINT ( 'NONE',  ( 1.453535542772391942, -31.06601413805603329, -2.750000000000000000 ) ) ;
#1394 = EDGE_CURVE ( 'NONE', #7772, #25535, #6551, .T. ) ;
#1395 = FACE_OUTER_BOUND ( 'NONE', #2684, .T. ) ;
#1396 =( GEOMETRIC_REPRESENTATION_CONTEXT ( 3 ) GLOBAL_UNCERTAINTY_ASSIGNED_CONTEXT ( ( #7042 ) ) GLOBAL_UNIT_ASSIGNED_CONTEXT ( ( #11728, #223, #13826 ) ) REPRESENTATION_CONTEXT ( 'NONE', 'WORKASPACE' ) );
#1397 = CARTESIAN_POINT ( 'NONE',  ( 3.735045420075836212E-15, 27.05312499938548498, 4.662447845253954171 ) ) ;
#1398 = CARTESIAN_POINT ( 'NONE',  ( -3.999999999999994671, 26.93124999877097281, 6.690598923241487306 ) ) ;
#1399 = CARTESIAN_POINT ( 'NONE',  ( 22.95237170627000367, 17.63997695035117985, 11.16877607737301226 ) ) ;
#1400 = CARTESIAN_POINT ( 'NONE',  ( 20.64088888413906986, 20.64088888413900236, 13.33755215474602984 ) ) ;
#1401 = CARTESIAN_POINT ( 'NONE',  ( -27.49048467073869517, -14.54246377227329212, -2.750000000000000000 ) ) ;
#1402 = CARTESIAN_POINT ( 'NONE',  ( 3.756430356250003655, 29.64062499938548356, 8.999999999999992895 ) ) ;
#1403 = CARTESIAN_POINT ( 'NONE',  ( 4.000000000000003553, -8.999999999999992895, 3.093749998770968457 ) ) ;
#1404 = CARTESIAN_POINT ( 'NONE',  ( 17.53391093317328142, 22.84630568909195958, 11.16877607737301048 ) ) ;
#1405 = CARTESIAN_POINT ( 'NONE',  ( 20.68849525807644696, 19.17274573022432094, 4.999999999999992895 ) ) ;
#1406 = ORIENTED_EDGE ( 'NONE', *, *, #3935, .F. ) ;
#1407 = CARTESIAN_POINT ( 'NONE',  ( 2.000000000000000888, 25.76874999877096784, 12.46410161513774817 ) ) ;
#1408 = CARTESIAN_POINT ( 'NONE',  ( 3.756430356250002323, 25.66562499938548569, 11.16877607737301226 ) ) ;
#1409 = CARTESIAN_POINT ( 'NONE',  ( 3.756430356249997882, -29.00312499938548072, 11.16877607737301226 ) ) ;
#1411 = ORIENTED_EDGE ( 'NONE', *, *, #13393, .F. ) ;
#1410 = CARTESIAN_POINT ( 'NONE',  ( 3.756430356250004099, 25.74062499938548854, 6.831223922626973533 ) ) ;
#1412 = CARTESIAN_POINT ( 'NONE',  ( 1.878215178125000939, 26.97812499938548569, 12.25316411605952283 ) ) ;
#1413 = ADVANCED_FACE ( 'NONE', ( #20019 ), #14291, .F. ) ;
#1414 = ORIENTED_EDGE ( 'NONE', *, *, #7433, .F. ) ;
#1415 = CARTESIAN_POINT ( 'NONE',  ( 1.878215178124998497, -28.14062499938548356, 12.25316411605951927 ) ) ;
#1416 = ORIENTED_EDGE ( 'NONE', *, *, #16411, .F. ) ;
#1417 = EDGE_LOOP ( 'NONE', ( #18226, #25662, #5734, #10746 ) ) ;
#1418 = FILL_AREA_STYLE_COLOUR ( '', #10543 ) ;
#1419 = CARTESIAN_POINT ( 'NONE',  ( -1.878215178124998275, 27.35312499938548925, 12.25316411605951927 ) ) ;
#1420 = CARTESIAN_POINT ( 'NONE',  ( 3.735045420075836212E-15, -4.662447845253954171, 2.053124999385483651 ) ) ;
#1421 = DIRECTION ( 'NONE',  ( 1.000000000000000000, 0.000000000000000000, 0.000000000000000000 ) ) ;
#1422 = ADVANCED_FACE ( 'NONE', ( #24079 ), #8392, .F. ) ;
#1423 = CARTESIAN_POINT ( 'NONE',  ( -27.10000000000000497, 0.6000000000000000888, 19.00000000000000000 ) ) ;
#1424 = FACE_OUTER_BOUND ( 'NONE', #1773, .T. ) ;
#1425 = DIRECTION ( 'NONE',  ( 0.000000000000000000, -1.000000000000000000, 0.000000000000000000 ) ) ;
#1426 = MECHANICAL_DESIGN_GEOMETRIC_PRESENTATION_REPRESENTATION (  '', ( #12709 ), #8113 ) ;
#1427 = CARTESIAN_POINT ( 'NONE',  ( -3.999999999999996447, 26.57500000000000284, 8.999999999999992895 ) ) ;
#1428 = DIRECTION ( 'NONE',  ( 0.9297764858882561212, 0.3681245526846659843, 0.000000000000000000 ) ) ;
#1429 = DIRECTION ( 'NONE',  ( -0.000000000000000000, -0.000000000000000000, 1.000000000000000000 ) ) ;
#1430 = CARTESIAN_POINT ( 'NONE',  ( 21.07620149587250680, 15.41934724638005605, 11.30940107675849760 ) ) ;
#1431 = ORIENTED_EDGE ( 'NONE', *, *, #11857, .F. ) ;
#1432 = DIRECTION ( 'NONE',  ( -0.8090169943749498938, -0.5877852522924696954, 0.000000000000000000 ) ) ;
#1433 = CARTESIAN_POINT ( 'NONE',  ( 3.756430356249997882, -28.66562499938548569, 11.16877607737301226 ) ) ;
#1434 = CARTESIAN_POINT ( 'NONE',  ( -3.756430356249995661, 25.44062499938548427, 6.831223922626973533 ) ) ;
#1435 = ADVANCED_FACE ( 'NONE', ( #14416 ), #20400, .T. ) ;
#1436 = CARTESIAN_POINT ( 'NONE',  ( 18.23451611984813425, 18.23451611984805609, 12.99999999999999112 ) ) ;
#1437 = CARTESIAN_POINT ( 'NONE',  ( -0.7500000000000001110, 20.00000000000000000, 18.19999999999999929 ) ) ;
#1438 = CARTESIAN_POINT ( 'NONE',  ( 20.91578934480144625, 19.40003981694932733, 12.99999999999999467 ) ) ;
#1439 = ORIENTED_EDGE ( 'NONE', *, *, #5014, .F. ) ;
#1440 = CARTESIAN_POINT ( 'NONE',  ( 3.999999999999996447, -26.96874999877096712, 8.999999999999992895 ) ) ;
#1441 = CARTESIAN_POINT ( 'NONE',  ( -23.46296185032681336, 19.82388608118453632, -6.500000000000000000 ) ) ;
#1443 = EDGE_LOOP ( 'NONE', ( #4353, #16270, #22985, #14828, #6396, #3255 ) ) ;
#1442 = DIRECTION ( 'NONE',  ( -0.000000000000000000, -0.000000000000000000, 1.000000000000000000 ) ) ;
#1444 = ADVANCED_FACE ( 'NONE', ( #12962 ), #2501, .F. ) ;
#1445 = VERTEX_POINT ( 'NONE', #14802 ) ;
#1446 = VERTEX_POINT ( 'NONE', #22777 ) ;
#1447 = ORIENTED_EDGE ( 'NONE', *, *, #54, .T. ) ;
#1448 = EDGE_LOOP ( 'NONE', ( #25041, #5384, #21791, #23680 ) ) ;
#1449 = DIRECTION ( 'NONE',  ( 1.000000000000000000, 0.000000000000000000, 0.000000000000000000 ) ) ;
#1450 =( BOUNDED_CURVE ( )  B_SPLINE_CURVE ( 2, ( #24955, #20651, #14896, #8622, #12803, #20777, #2733, #5091, #2856 ),
 .UNSPECIFIED., .F., .F. ) 
 B_SPLINE_CURVE_WITH_KNOTS ( ( 3, 2, 2, 2, 3 ),
 ( 0.3750000000000000000, 0.3833333333333333592, 0.4000000000000000222, 0.4166666666666666852, 0.4250000000000000444 ),
 .UNSPECIFIED. ) 
 CURVE ( )  GEOMETRIC_REPRESENTATION_ITEM ( )  RATIONAL_B_SPLINE_CURVE ( ( 0.9330127018922194093, 0.9330127018922194093, 1.000000000000000000, 0.8660254037844387076, 1.000000000000000000, 0.8660254037844387076, 1.000000000000000000, 0.9330127018922191873, 0.9330127018922194093 ) ) 
 REPRESENTATION_ITEM ( '' )  );
#1451 = CARTESIAN_POINT ( 'NONE',  ( -20.78941499438242246, -22.67092431280570963, -6.500000000000000000 ) ) ;
#1452 = FACE_OUTER_BOUND ( 'NONE', #21387, .T. ) ;
#1453 = CARTESIAN_POINT ( 'NONE',  ( -3.756430356249995661, -6.831223922626973533, 2.578124999385481342 ) ) ;
#1454 = CARTESIAN_POINT ( 'NONE',  ( 4.000000000000003553, -8.999999999999992895, 2.643749998770966059 ) ) ;
#1455 = SURFACE_SIDE_STYLE ('',( #19360 ) ) ;
#1456 = CARTESIAN_POINT ( 'NONE',  ( 3.756430356250003655, 28.85312499938548569, 8.999999999999992895 ) ) ;
#1457 = DIRECTION ( 'NONE',  ( 1.000000000000000000, 0.000000000000000000, 0.000000000000000000 ) ) ;
#1458 = CARTESIAN_POINT ( 'NONE',  ( 1.071796769724494558, 28.63615380933863364, 4.999999999999992895 ) ) ;
#1459 = CARTESIAN_POINT ( 'NONE',  ( 2.000000000000000888, -12.46410161513774817, 2.174999999999999822 ) ) ;
#1460 = CARTESIAN_POINT ( 'NONE',  ( -4.000000000000001776, -25.80624999877096926, 11.30940107675849760 ) ) ;
#1461 = FACE_OUTER_BOUND ( 'NONE', #21531, .T. ) ;
#1462 = CARTESIAN_POINT ( 'NONE',  ( 18.87533163942939041, 21.70375876417550032, 5.535898384862237620 ) ) ;
#1463 = CARTESIAN_POINT ( 'NONE',  ( 3.999999999999996003, -26.93124999877096926, 6.690598923241487306 ) ) ;
#1464 = CARTESIAN_POINT ( 'NONE',  ( 2.672651547586948120E-15, -13.33755215474603162, 4.190624999385483385 ) ) ;
#1465 = CYLINDRICAL_SURFACE ( 'NONE', #331, 4.000000000000000000 ) ;
#1466 = ADVANCED_FACE ( 'NONE', ( #12569 ), #4854, .T. ) ;
#1467 = CARTESIAN_POINT ( 'NONE',  ( 0.000000000000000000, 0.000000000000000000, -6.500000000000000000 ) ) ;
#1468 = ORIENTED_EDGE ( 'NONE', *, *, #14358, .T. ) ;
#1469 = DIRECTION ( 'NONE',  ( 1.000000000000000000, 0.000000000000000000, 0.000000000000000000 ) ) ;
#1470 = ORIENTED_EDGE ( 'NONE', *, *, #18126, .F. ) ;
#1471 = ADVANCED_FACE ( 'NONE', ( #20804 ), #3026, .T. ) ;
#1472 = ORIENTED_EDGE ( 'NONE', *, *, #300, .F. ) ;
#1473 = CARTESIAN_POINT ( 'NONE',  ( 29.57785765677931167, 9.610428525060783045, -6.500000000000000000 ) ) ;
#1474 = ORIENTED_EDGE ( 'NONE', *, *, #20091, .T. ) ;
#1475 = CARTESIAN_POINT ( 'NONE',  ( -3.756430356250002323, -27.91562499938548569, 11.16877607737301226 ) ) ;
#1476 = ORIENTED_EDGE ( 'NONE', *, *, #12495, .F. ) ;
#1477 = CARTESIAN_POINT ( 'NONE',  ( 4.000000000000003553, 26.83749999999999503, 6.690598923241489970 ) ) ;
#1478 = ORIENTED_EDGE ( 'NONE', *, *, #8035, .F. ) ;
#1479 = EDGE_CURVE ( 'NONE', #12855, #15503, #7340, .T. ) ;
#1480 = CARTESIAN_POINT ( 'NONE',  ( 3.752267015613588906E-15, 28.26250000000000284, 4.381197846482986158 ) ) ;
#1481 = CARTESIAN_POINT ( 'NONE',  ( 3.469446951953614189E-15, 46.00000000000000000, 8.999999999999992895 ) ) ;
#1482 = CARTESIAN_POINT ( 'NONE',  ( -3.999999999999995559, 26.53750000000000142, 6.690598923241487306 ) ) ;
#1483 = CARTESIAN_POINT ( 'NONE',  ( -19.43607991388954304, 24.27856662945528399, -6.500000000000000000 ) ) ;
#1484 = CARTESIAN_POINT ( 'NONE',  ( 16.87327180006579752, 19.52946917802510285, 5.746835883940462963 ) ) ;
#1485 = CARTESIAN_POINT ( 'NONE',  ( 3.469446951953614189E-15, -8.999999999999992895, 18.00000000000000000 ) ) ;
#1486 = ADVANCED_FACE ( 'NONE', ( #14531 ), #16900, .T. ) ;
#1487 = CARTESIAN_POINT ( 'NONE',  ( 4.000000000000003553, 26.83749999999999503, 6.690598923241489970 ) ) ;
#1488 = CARTESIAN_POINT ( 'NONE',  ( 21.49396397007274473, 16.18156921415393157, 6.831223922626973533 ) ) ;
#1489 = CARTESIAN_POINT ( 'NONE',  ( -3.137519842735244810E-15, 26.85624999877096641, 4.999999999999991118 ) ) ;
#1490 = VECTOR ( 'NONE', #192, 1000.000000000000000 ) ;
#1491 = ORIENTED_EDGE ( 'NONE', *, *, #14009, .T. ) ;
#1492 = VERTEX_POINT ( 'NONE', #8776 ) ;
#1493 = CARTESIAN_POINT ( 'NONE',  ( 2.003086131649545506E-15, 28.88124999877097210, 13.61880215351699874 ) ) ;
#1494 = CARTESIAN_POINT ( 'NONE',  ( 3.756430356249997438, -29.45312499938548356, 11.16877607737301048 ) ) ;
#1495 = ORIENTED_EDGE ( 'NONE', *, *, #8498, .T. ) ;
#1496 = DIRECTION ( 'NONE',  ( 0.000000000000000000, 0.000000000000000000, 1.000000000000000000 ) ) ;
#1497 = CARTESIAN_POINT ( 'NONE',  ( -1.878215178124995832, 28.55312499938548498, 5.746835883940462963 ) ) ;
#1498 = CARTESIAN_POINT ( 'NONE',  ( 1.453535542772518951, -31.06601413805602618, 1.000000000000000000 ) ) ;
#1499 = EDGE_LOOP ( 'NONE', ( #15805, #18809, #521, #10617 ) ) ;
#1500 = EDGE_CURVE ( 'NONE', #6543, #19882, #20943, .T. ) ;
#1501 = ORIENTED_EDGE ( 'NONE', *, *, #9500, .F. ) ;
#1502 = CARTESIAN_POINT ( 'NONE',  ( 4.000000000000049738, -6.690598923241514839, 4.087499999999997691 ) ) ;
#1503 = VERTEX_POINT ( 'NONE', #6819 ) ;
#1504 = EDGE_CURVE ( 'NONE', #11855, #2116, #230, .T. ) ;
#1505 = CARTESIAN_POINT ( 'NONE',  ( 1.878215178124995832, -28.10312499938548569, 5.746835883940462963 ) ) ;
#1506 = CARTESIAN_POINT ( 'NONE',  ( 1.878215178125004048, 25.66562499938548569, 5.746835883940462963 ) ) ;
#1507 = CARTESIAN_POINT ( 'NONE',  ( 3.756430356250002323, 27.80312499938548854, 11.16877607737301403 ) ) ;
#1508 = EDGE_CURVE ( 'NONE', #21865, #6673, #1909, .T. ) ;
#1509 = VECTOR ( 'NONE', #25750, 1000.000000000000000 ) ;
#1510 = CARTESIAN_POINT ( 'NONE',  ( 31.00322564728513086, -2.451530025009243108, -6.500000000000000000 ) ) ;
#1511 = CARTESIAN_POINT ( 'NONE',  ( 6.009258394948636914E-15, 26.01250000000000284, 4.381197846482986158 ) ) ;
#1512 = CARTESIAN_POINT ( 'NONE',  ( -1.878215178124998497, 29.49062499938548498, 12.25316411605951927 ) ) ;
#1513 = CARTESIAN_POINT ( 'NONE',  ( 0.000000000000000000, 0.000000000000000000, 1.000000000000000000 ) ) ;
#1514 = CARTESIAN_POINT ( 'NONE',  ( -3.918623196469422698, 38.49999999999999289, 13.54361004533748059 ) ) ;
#1515 = CARTESIAN_POINT ( 'NONE',  ( 1.878215178125004048, 26.56562499938548427, 5.746835883940462963 ) ) ;
#1516 = CARTESIAN_POINT ( 'NONE',  ( 4.000000000000003553, 25.00000000000000000, 8.999999999999992895 ) ) ;
#1517 = CARTESIAN_POINT ( 'NONE',  ( 16.59933168835424411, 22.25618593784655630, 8.999999999999992895 ) ) ;
#1518 = CARTESIAN_POINT ( 'NONE',  ( 21.04090992281141581, 18.38471254485196837, 12.25316411605952283 ) ) ;
#1519 = CYLINDRICAL_SURFACE ( 'NONE', #14271, 31.10000000000000142 ) ;
#1520 = CARTESIAN_POINT ( 'NONE',  ( -0.7500000000000001110, 9.184850993605150903E-17, 15.00000000000000178 ) ) ;
#1521 = CARTESIAN_POINT ( 'NONE',  ( 23.52603154635960436, 18.61577656318150176, 6.996763648122161783 ) ) ;
#1522 = CARTESIAN_POINT ( 'NONE',  ( 21.99777755166815751, 16.68538279574934435, 11.16877607737301403 ) ) ;
#1523 = DIRECTION ( 'NONE',  ( 1.000000000000000000, 0.000000000000000000, 0.000000000000000000 ) ) ;
#1524 = VERTEX_POINT ( 'NONE', #6549 ) ;
#1525 = CARTESIAN_POINT ( 'NONE',  ( -3.999999999999996003, 25.58124999877097139, 6.690598923241487306 ) ) ;
#1526 = CARTESIAN_POINT ( 'NONE',  ( 3.999999999999996447, -26.57500000000000284, 8.999999999999992895 ) ) ;
#1528 = VERTEX_POINT ( 'NONE', #940 ) ;
#1527 = FACE_OUTER_BOUND ( 'NONE', #671, .T. ) ;
#1529 = CARTESIAN_POINT ( 'NONE',  ( 3.756430356250003211, 26.19062499938548783, 6.831223922626973533 ) ) ;
#1530 = CARTESIAN_POINT ( 'NONE',  ( 1.999999999999998224, -29.74374999877096926, 12.46410161513774639 ) ) ;
#1531 = ORIENTED_EDGE ( 'NONE', *, *, #3720, .T. ) ;
#1532 = CARTESIAN_POINT ( 'NONE',  ( -3.756430356250003655, -27.84062499938548640, 8.999999999999992895 ) ) ;
#1533 = VERTEX_POINT ( 'NONE', #18708 ) ;
#1534 = PRODUCT_DEFINITION_SHAPE ( 'NONE', 'NONE',  #17976 ) ;
#1535 = ORIENTED_EDGE ( 'NONE', *, *, #10759, .F. ) ;
#1536 = EDGE_CURVE ( 'NONE', #4330, #17764, #6946, .T. ) ;
#1537 = CARTESIAN_POINT ( 'NONE',  ( 19.74676196587764210, 22.58567065652198735, 12.46960170373642107 ) ) ;
#1538 = CARTESIAN_POINT ( 'NONE',  ( 1.878215178125003382, 29.67812499938549209, 12.25316411605952283 ) ) ;
#1539 = ADVANCED_FACE ( 'NONE', ( #20678 ), #14668, .T. ) ;
#1540 = LINE ( 'NONE', #25464, #24379 ) ;
#1541 = EDGE_CURVE ( 'NONE', #17200, #10079, #20708, .T. ) ;
#1542 = CARTESIAN_POINT ( 'NONE',  ( 3.735045420075836212E-15, -4.662447845253954171, 3.965624999385486404 ) ) ;
#1543 =( LENGTH_UNIT ( ) NAMED_UNIT ( * ) SI_UNIT ( .MILLI., .METRE. ) );
#1544 = DIRECTION ( 'NONE',  ( 0.000000000000000000, 0.000000000000000000, 1.000000000000000000 ) ) ;
#1545 = CARTESIAN_POINT ( 'NONE',  ( 4.000000000000005329, 26.83750000000000213, 6.690598923241489970 ) ) ;
#1546 = DIRECTION ( 'NONE',  ( 1.000000000000000000, 0.000000000000000000, 0.000000000000000000 ) ) ;
#1547 = CARTESIAN_POINT ( 'NONE',  ( -28.34936733434208733, -12.78762572734038727, 1.000000000000000000 ) ) ;
#1548 = CYLINDRICAL_SURFACE ( 'NONE', #6201, 31.10000000000000142 ) ;
#1549 = PLANE ( 'NONE',  #5781 ) ;
#1550 = CARTESIAN_POINT ( 'NONE',  ( 16.64794527869176122, 19.47637240343788179, 5.535898384862237620 ) ) ;
#1551 = ORIENTED_EDGE ( 'NONE', *, *, #2804, .T. ) ;
#1552 = LINE ( 'NONE', #23523, #5088 ) ;
#1553 = CARTESIAN_POINT ( 'NONE',  ( 9.133673601486252736, -29.72853858738288935, -2.750000000000000000 ) ) ;
#1554 = CARTESIAN_POINT ( 'NONE',  ( -3.756430356249997882, 26.86562499938548498, 11.16877607737301226 ) ) ;
#1555 = DIRECTION ( 'NONE',  ( 0.000000000000000000, -0.000000000000000000, 1.000000000000000000 ) ) ;
#1556 = CARTESIAN_POINT ( 'NONE',  ( 3.834746474454188013E-15, 27.36250000000000426, 4.999999999999992006 ) ) ;
#1557 = CARTESIAN_POINT ( 'NONE',  ( 3.918623196469491976, 38.49999999999999289, 13.54361004533742907 ) ) ;
#1558 = ORIENTED_EDGE ( 'NONE', *, *, #2307, .F. ) ;
#1559 = DIRECTION ( 'NONE',  ( 0.000000000000000000, 1.000000000000000000, 0.000000000000000000 ) ) ;
#1560 = CYLINDRICAL_SURFACE ( 'NONE', #1671, 31.10000000000000142 ) ;
#1562 = ORIENTED_EDGE ( 'NONE', *, *, #23060, .F. ) ;
#1561 = CARTESIAN_POINT ( 'NONE',  ( 10.08469938919487419, 29.41953157733095026, 1.000000000000000000 ) ) ;
#1563 = ORIENTED_EDGE ( 'NONE', *, *, #22830, .F. ) ;
#1564 = ORIENTED_EDGE ( 'NONE', *, *, #24964, .T. ) ;
#1565 = ORIENTED_EDGE ( 'NONE', *, *, #10538, .F. ) ;
#1566 = ORIENTED_EDGE ( 'NONE', *, *, #6970, .T. ) ;
#1567 = EDGE_CURVE ( 'NONE', #21040, #583, #8647, .T. ) ;
#1568 = CARTESIAN_POINT ( 'NONE',  ( 0.000000000000000000, 0.000000000000000000, 1.000000000000000000 ) ) ;
#1569 = CYLINDRICAL_SURFACE ( 'NONE', #24050, 31.10000000000000142 ) ;
#1570 = EDGE_CURVE ( 'NONE', #23781, #19322, #259, .T. ) ;
#1571 = CARTESIAN_POINT ( 'NONE',  ( -3.999999999999996447, 27.92500000000000426, 8.999999999999992895 ) ) ;
#1572 = CARTESIAN_POINT ( 'NONE',  ( 1.878215178125004048, -5.746835883940462963, 2.015624999385484450 ) ) ;
#1573 = CARTESIAN_POINT ( 'NONE',  ( 2.620986760973688460E-15, -13.61880215351699874, 1.181249998770967258 ) ) ;
#1574 = CARTESIAN_POINT ( 'NONE',  ( 3.756430356250004099, 28.89062499938548356, 6.831223922626973533 ) ) ;
#1575 = EDGE_CURVE ( 'NONE', #17398, #7608, #650, .T. ) ;
#1576 = LINE ( 'NONE', #19611, #1274 ) ;
#1577 = CARTESIAN_POINT ( 'NONE',  ( -25.45105997952938637, -17.87326343783915306, -6.500000000000000000 ) ) ;
#1578 = CARTESIAN_POINT ( 'NONE',  ( 4.000000000000003553, -8.999999999999992895, 1.799999999999999600 ) ) ;
#1579 =( REPRESENTATION_RELATIONSHIP ('NONE','NONE', #25031, #19829 ) REPRESENTATION_RELATIONSHIP_WITH_TRANSFORMATION ( #10096 )SHAPE_REPRESENTATION_RELATIONSHIP( ) );
#1580 = DIRECTION ( 'NONE',  ( 0.9685831611286337406, 0.2486898871648445808, 0.000000000000000000 ) ) ;
#1581 = CARTESIAN_POINT ( 'NONE',  ( -23.46296185032681336, 19.82388608118453632, -6.500000000000000000 ) ) ;
#1582 = DIRECTION ( 'NONE',  ( 1.000000000000000000, 0.000000000000000000, 0.000000000000000000 ) ) ;
#1583 =( BOUNDED_CURVE ( )  B_SPLINE_CURVE ( 2, ( #2616, #8892, #23007, #22623, #20520, #20913, #10828, #18822, #12408 ),
 .UNSPECIFIED., .F., .F. ) 
 B_SPLINE_CURVE_WITH_KNOTS ( ( 3, 2, 2, 2, 3 ),
 ( 0.8750000000000000000, 0.8833333333333333037, 0.9000000000000000222, 0.9166666666666666297, 0.9250000000000000444 ),
 .UNSPECIFIED. ) 
 CURVE ( )  GEOMETRIC_REPRESENTATION_ITEM ( )  RATIONAL_B_SPLINE_CURVE ( ( 0.9330127018922194093, 0.9330127018922194093, 1.000000000000000000, 0.8660254037844387076, 1.000000000000000000, 0.8660254037844387076, 1.000000000000000000, 0.9330127018922189652, 0.9330127018922194093 ) ) 
 REPRESENTATION_ITEM ( '' )  );
#1584 = CARTESIAN_POINT ( 'NONE',  ( -4.000000000000003553, -26.33124999877097139, 6.690598923241489970 ) ) ;
#1585 = CARTESIAN_POINT ( 'NONE',  ( 3.756430356250002323, 29.26562499938548356, 11.16877607737301226 ) ) ;
#1586 = DIRECTION ( 'NONE',  ( -0.5358267949789882190, 0.8443279255020205154, 0.000000000000000000 ) ) ;
#1587 = VECTOR ( 'NONE', #14038, 1000.000000000000000 ) ;
#1588 = DIRECTION ( 'NONE',  ( 0.000000000000000000, 0.000000000000000000, 1.000000000000000000 ) ) ;
#1589 = CARTESIAN_POINT ( 'NONE',  ( 4.000000000000003553, -8.999999999999992895, 3.993749998770966592 ) ) ;
#1590 = VERTEX_POINT ( 'NONE', #18171 ) ;
#1591 = DIRECTION ( 'NONE',  ( 1.000000000000000000, 0.000000000000000000, -0.000000000000000000 ) ) ;
#1592 = ORIENTED_EDGE ( 'NONE', *, *, #22431, .T. ) ;
#1593 =( BOUNDED_CURVE ( )  B_SPLINE_CURVE ( 2, ( #15644, #17088, #5190, #1398, #23610, #7280, #23108, #9485, #15257 ),
 .UNSPECIFIED., .F., .F. ) 
 B_SPLINE_CURVE_WITH_KNOTS ( ( 3, 2, 2, 2, 3 ),
 ( 0.3250000000000000111, 0.3333333333333333148, 0.3499999999999999778, 0.3666666666666666408, 0.3750000000000000000 ),
 .UNSPECIFIED. ) 
 CURVE ( )  GEOMETRIC_REPRESENTATION_ITEM ( )  RATIONAL_B_SPLINE_CURVE ( ( 0.9330127018922194093, 0.9330127018922196314, 1.000000000000000000, 0.8660254037844387076, 1.000000000000000000, 0.8660254037844387076, 1.000000000000000000, 0.9330127018922194093, 0.9330127018922194093 ) ) 
 REPRESENTATION_ITEM ( '' )  );
#1594 = EDGE_LOOP ( 'NONE', ( #24309, #8224, #19587, #15571 ) ) ;
#1595 = CARTESIAN_POINT ( 'NONE',  ( 11.44867358849329619, -28.91604871112469510, -6.500000000000000000 ) ) ;
#1597 = ORIENTED_EDGE ( 'NONE', *, *, #18674, .T. ) ;
#1596 = CIRCLE ( 'NONE', #343, 0.5000000000000002220 ) ;
#1598 = CARTESIAN_POINT ( 'NONE',  ( -1.878215178125004048, -27.12812499938548783, 5.746835883940462963 ) ) ;
#1599 = ORIENTED_EDGE ( 'NONE', *, *, #15919, .F. ) ;
#1600 = ORIENTED_EDGE ( 'NONE', *, *, #24972, .T. ) ;
#1601 = DIRECTION ( 'NONE',  ( 0.000000000000000000, 0.000000000000000000, 1.000000000000000000 ) ) ;
#1602 = VERTEX_POINT ( 'NONE', #6000 ) ;
#1603 = CARTESIAN_POINT ( 'NONE',  ( 4.000000000000003553, 26.38750000000000284, 6.690598923241489970 ) ) ;
#1604 = VECTOR ( 'NONE', #22634, 1000.000000000000000 ) ;
#1605 = ADVANCED_FACE ( 'NONE', ( #8220 ), #13982, .F. ) ;
#1606 = CARTESIAN_POINT ( 'NONE',  ( 2.900000000000003464, -8.999999999999992895, 25.00000000000000000 ) ) ;
#1607 = CARTESIAN_POINT ( 'NONE',  ( 19.60447174239884305, 22.26066912035814127, 12.25316411605951927 ) ) ;
#1608 = CARTESIAN_POINT ( 'NONE',  ( 3.469446951953614189E-15, -8.999999999999992895, 18.00000000000000000 ) ) ;
#1609 = AXIS2_PLACEMENT_3D ( 'NONE', #14552, #22398, #2146 ) ;
#1610 = CARTESIAN_POINT ( 'NONE',  ( -3.999999999999997335, 28.86250000000000071, 11.30940107675849404 ) ) ;
#1611 = EDGE_CURVE ( 'NONE', #2153, #19796, #22459, .T. ) ;
#1612 = CARTESIAN_POINT ( 'NONE',  ( 23.08495422774248240, 17.77255947182365503, 6.831223922626973533 ) ) ;
#1613 = CARTESIAN_POINT ( 'NONE',  ( 2.000000000000005329, 28.22500000000000497, 5.535898384862238508 ) ) ;
#1614 = VERTEX_POINT ( 'NONE', #16077 ) ;
#1615 = EDGE_LOOP ( 'NONE', ( #1947, #4726, #1491, #22145 ) ) ;
#1616 = CARTESIAN_POINT ( 'NONE',  ( 3.756430356250000546, 26.56562499938548783, 11.16877607737301226 ) ) ;
#1618 = EDGE_LOOP ( 'NONE', ( #2456, #10455, #25171, #2324 ) ) ;
#1617 = AXIS2_PLACEMENT_3D ( 'NONE', #19728, #19843, #5727 ) ;
#1619 = CARTESIAN_POINT ( 'NONE',  ( -3.834746474454188013E-15, -27.81249999999999645, 4.999999999999992006 ) ) ;
#1620 = AXIS2_PLACEMENT_3D ( 'NONE', #360, #1937, #4144 ) ;
#1621 = CARTESIAN_POINT ( 'NONE',  ( 3.756430356250004099, 27.09062499938548285, 6.831223922626973533 ) ) ;
#1622 = DIRECTION ( 'NONE',  ( 1.000000000000000000, 0.000000000000000000, 0.000000000000000000 ) ) ;
#1623 = ORIENTED_EDGE ( 'NONE', *, *, #8353, .F. ) ;
#1624 = ORIENTED_EDGE ( 'NONE', *, *, #20661, .F. ) ;
#1625 = CARTESIAN_POINT ( 'NONE',  ( 1.071796769724495224, 25.09240381056766722, 4.999999999999992895 ) ) ;
#1626 = CIRCLE ( 'NONE', #4553, 31.10000000000000142 ) ;
#1627 = VERTEX_POINT ( 'NONE', #252 ) ;
#1628 = EDGE_CURVE ( 'NONE', #22817, #8694, #10042, .T. ) ;
#1629 = CARTESIAN_POINT ( 'NONE',  ( 3.481718437949647083, 38.92511481668519480, 4.645898033752395406 ) ) ;
#1630 = CARTESIAN_POINT ( 'NONE',  ( -3.756430356249996994, 25.36562499938548498, 8.999999999999992895 ) ) ;
#1631 = CARTESIAN_POINT ( 'NONE',  ( 3.756430356250003211, 28.74062499938548498, 8.999999999999992895 ) ) ;
#1632 = CARTESIAN_POINT ( 'NONE',  ( 25.16042852506090810, 18.28012134629586072, 1.000000000000000000 ) ) ;
#1633 = CARTESIAN_POINT ( 'NONE',  ( 4.000000000000005329, 26.38750000000000639, 6.690598923241489970 ) ) ;
#1634 = EDGE_CURVE ( 'NONE', #16116, #24580, #512, .T. ) ;
#1635 = VECTOR ( 'NONE', #16499, 999.9999999999998863 ) ;
#1636 = CARTESIAN_POINT ( 'NONE',  ( -3.756430356249996994, 28.96562499938548285, 8.999999999999992895 ) ) ;
#1637 = ADVANCED_FACE ( 'NONE', ( #24301 ), #1015, .F. ) ;
#1638 = LINE ( 'NONE', #17462, #24206 ) ;
#1639 = CIRCLE ( 'NONE', #19592, 31.10000000000000142 ) ;
#1640 = CARTESIAN_POINT ( 'NONE',  ( -3.999999999999997335, 27.51250000000000284, 11.30940107675849404 ) ) ;
#1641 = CARTESIAN_POINT ( 'NONE',  ( -1.878215178124998497, 28.14062499938548356, 12.25316411605951927 ) ) ;
#1642 = AXIS2_PLACEMENT_3D ( 'NONE', #24457, #22361, #22882 ) ;
#1643 = CARTESIAN_POINT ( 'NONE',  ( 3.878215178125003604, 29.82343749907822783, 8.999999999999992895 ) ) ;
#1644 = CARTESIAN_POINT ( 'NONE',  ( 16.28113363682029657, 21.93798788631260877, 8.999999999999992895 ) ) ;
#1645 = CARTESIAN_POINT ( 'NONE',  ( 22.13036007314063625, 16.81796531722181598, 6.831223922626973533 ) ) ;
#1646 = EDGE_CURVE ( 'NONE', #3229, #12524, #24873, .T. ) ;
#1647 = DIRECTION ( 'NONE',  ( 1.000000000000000000, 0.000000000000000000, 0.000000000000000000 ) ) ;
#1648 = CARTESIAN_POINT ( 'NONE',  ( 3.469446951953614189E-15, 30.00000000000000355, 8.999999999999992895 ) ) ;
#1649 = CARTESIAN_POINT ( 'NONE',  ( 23.60239120520362022, 18.51856749399161473, 7.226316032987424975 ) ) ;
#1650 = DIRECTION ( 'NONE',  ( 1.000000000000000000, 0.000000000000000000, 0.000000000000000000 ) ) ;
#1651 = VECTOR ( 'NONE', #15719, 1000.000000000000000 ) ;
#1652 = CARTESIAN_POINT ( 'NONE',  ( 2.000000000000000000, 25.76874999877097139, 12.46410161513774817 ) ) ;
#1653 = EDGE_LOOP ( 'NONE', ( #16304, #8249, #22495, #7437 ) ) ;
#1654 = CARTESIAN_POINT ( 'NONE',  ( -3.999999999999996447, 26.06874999877096855, 8.999999999999992895 ) ) ;
#1655 = CARTESIAN_POINT ( 'NONE',  ( -3.752267015613588906E-15, -25.56250000000000000, 4.381197846482986158 ) ) ;
#1657 = VERTEX_POINT ( 'NONE', #16220 ) ;
#1656 = CARTESIAN_POINT ( 'NONE',  ( 0.000000000000000000, 0.000000000000000000, -6.500000000000000000 ) ) ;
#1658 = CARTESIAN_POINT ( 'NONE',  ( -3.756430356249996105, 26.34062499938548285, 6.831223922626973533 ) ) ;
#1659 = CIRCLE ( 'NONE', #10826, 31.10000000000000142 ) ;
#1660 = ADVANCED_FACE ( 'NONE', ( #10583 ), #20663, .F. ) ;
#1661 = DIRECTION ( 'NONE',  ( 0.000000000000000000, -1.000000000000000000, 0.000000000000000000 ) ) ;
#1662 = AXIS2_PLACEMENT_3D ( 'NONE', #11194, #1271, #8727 ) ;
#1663 = ORIENTED_EDGE ( 'NONE', *, *, #22246, .F. ) ;
#1664 = CARTESIAN_POINT ( 'NONE',  ( -8.217531866531306406, -29.99470236596026851, 1.000000000000000000 ) ) ;
#1665 = VERTEX_POINT ( 'NONE', #2239 ) ;
#1666 = VERTEX_POINT ( 'NONE', #16745 ) ;
#1667 = SURFACE_STYLE_FILL_AREA ( #7802 ) ;
#1668 = CARTESIAN_POINT ( 'NONE',  ( 3.756430356250004987, 25.14062499938548356, 8.999999999999992895 ) ) ;
#1669 = AXIS2_PLACEMENT_3D ( 'NONE', #5031, #11432, #22947 ) ;
#1670 = CARTESIAN_POINT ( 'NONE',  ( -3.756430356249997438, -11.16877607737301048, 0.4031249993854806868 ) ) ;
#1671 = AXIS2_PLACEMENT_3D ( 'NONE', #23266, #1166, #21180 ) ;
#1672 = DIRECTION ( 'NONE',  ( 1.000000000000000000, 0.000000000000000000, 0.000000000000000000 ) ) ;
#1673 = SURFACE_SIDE_STYLE ('',( #11477 ) ) ;
#1674 = CARTESIAN_POINT ( 'NONE',  ( 16.23990935651698564, -26.52310962334756184, -6.500000000000000000 ) ) ;
#1675 = VECTOR ( 'NONE', #6954, 1000.000000000000000 ) ;
#1676 = CARTESIAN_POINT ( 'NONE',  ( 4.000000000000005329, 29.05000000000000426, 8.999999999999992895 ) ) ;
#1677 = CARTESIAN_POINT ( 'NONE',  ( -1.499999999999998224, -10.49999999999999289, 30.00000000000000355 ) ) ;
#1678 = DIRECTION ( 'NONE',  ( 0.000000000000000000, 0.000000000000000000, 1.000000000000000000 ) ) ;
#1679 = CYLINDRICAL_SURFACE ( 'NONE', #11711, 0.7500000000000001110 ) ;
#1680 = CARTESIAN_POINT ( 'NONE',  ( 20.75150184982686596, 15.43910709390805280, 8.999999999999992895 ) ) ;
#1681 = CARTESIAN_POINT ( 'NONE',  ( 30.12293631110040693, -7.734255490827107948, 1.000000000000000000 ) ) ;
#1682 = EDGE_CURVE ( 'NONE', #8556, #23396, #14649, .T. ) ;
#1683 = VERTEX_POINT ( 'NONE', #22237 ) ;
#1684 = DIRECTION ( 'NONE',  ( 0.000000000000000000, 0.000000000000000000, 1.000000000000000000 ) ) ;
#1685 = CARTESIAN_POINT ( 'NONE',  ( 3.756430356249996994, -29.52812499938548640, 8.999999999999992895 ) ) ;
#1686 = CARTESIAN_POINT ( 'NONE',  ( -3.756430356249997882, 27.76562499938549067, 11.16877607737301226 ) ) ;
#1688 = EDGE_CURVE ( 'NONE', #1445, #19775, #10234, .T. ) ;
#1687 = CIRCLE ( 'NONE', #2119, 31.10000000000000142 ) ;
#1689 = CARTESIAN_POINT ( 'NONE',  ( 4.000000000000034639, -6.690598923241508622, 2.287499999999995648 ) ) ;
#1690 = DIRECTION ( 'NONE',  ( 0.000000000000000000, 1.000000000000000000, 0.000000000000000000 ) ) ;
#1691 = DIRECTION ( 'NONE',  ( 0.000000000000000000, 0.000000000000000000, 1.000000000000000000 ) ) ;
#1692 = ORIENTED_EDGE ( 'NONE', *, *, #9696, .F. ) ;
#1693 = DIRECTION ( 'NONE',  ( 0.000000000000000000, 0.000000000000000000, 1.000000000000000000 ) ) ;
#1694 = CARTESIAN_POINT ( 'NONE',  ( -23.46296185032722548, -19.82388608118403539, -6.500000000000000000 ) ) ;
#1696 = EDGE_LOOP ( 'NONE', ( #4976, #21317, #11139, #14311 ) ) ;
#1695 = CARTESIAN_POINT ( 'NONE',  ( 6.972266317189432034E-15, 28.65624999877097423, 4.999999999999992006 ) ) ;
#1697 = EDGE_CURVE ( 'NONE', #25550, #4816, #12338, .T. ) ;
#1698 = ORIENTED_EDGE ( 'NONE', *, *, #1206, .F. ) ;
#1699 = CIRCLE ( 'NONE', #20903, 0.4999999999999992784 ) ;
#1700 = ORIENTED_EDGE ( 'NONE', *, *, #14006, .F. ) ;
#1701 = VERTEX_POINT ( 'NONE', #24190 ) ;
#1702 = ORIENTED_EDGE ( 'NONE', *, *, #22026, .T. ) ;
#1703 = DIRECTION ( 'NONE',  ( 1.000000000000000000, 0.000000000000000000, 0.000000000000000000 ) ) ;
#1704 = DIRECTION ( 'NONE',  ( -0.000000000000000000, -0.000000000000000000, 1.000000000000000000 ) ) ;
#1705 = VECTOR ( 'NONE', #15383, 1000.000000000000000 ) ;
#1706 = DIRECTION ( 'NONE',  ( 1.000000000000000000, 0.000000000000000000, 0.000000000000000000 ) ) ;
#1707 = CLOSED_SHELL ( 'NONE', ( #20653, #11784, #20616, #2004, #13663, #21351, #1930, #21195, #2430, #23617, #4209, #4037, #21887, #11701, #10287, #9179, #24063, #13901, #21749, #1210, #17984, #25388, #6940, #22389, #10182, #2011, #24637, #20740, #8165, #15835, #14762, #17627, #23412, #16719, #4571, #6059, #1064, #3906, #4390, #16275, #15401, #13456, #9685, #11222, #5105, #18015, #16983, #19187, #13692, #1977, #5001, #19635, #17079, #20177, #1150, #5131, #3102, #676, #7145, #24903, #14109, #598, #13778, #20832, #14216, #713, #16143, #20555, #11466, #65, #12736, #9369, #6134, #426, #9609, #2958, #3530, #10783, #16931, #18200, #24170, #24494, #8665, #3823, #18770, #25765, #8141, #12180, #7903, #12881, #22087, #1905, #15163, #8674, #4136, #11422, #9408, #7262, #7190, #1637, #14444, #2194, #25555, #20558, #6885, #5485, #9859, #19759, #18095, #19399, #3559, #16200, #11747, #22253, #20841, #17559, #21319 ) ) ;
#1708 = CARTESIAN_POINT ( 'NONE',  ( 23.80283954968513171, 18.26064280072889190, 9.928636277907715524 ) ) ;
#1709 = VECTOR ( 'NONE', #10698, 1000.000000000000000 ) ;
#1710 = CARTESIAN_POINT ( 'NONE',  ( -3.756430356249996994, -8.999999999999992895, 3.965624999385481519 ) ) ;
#1711 = CARTESIAN_POINT ( 'NONE',  ( -1.999999999999995781, -5.535898384862237620, 0.9937499987709673688 ) ) ;
#1712 = FILL_AREA_STYLE_COLOUR ( '', #7654 ) ;
#1713 = CARTESIAN_POINT ( 'NONE',  ( -1.878215178124998497, 29.15312499938548640, 12.25316411605951927 ) ) ;
#1714 = DIRECTION ( 'NONE',  ( 1.000000000000000000, 0.000000000000000000, 0.000000000000000000 ) ) ;
#1715 = VECTOR ( 'NONE', #7862, 1000.000000000000000 ) ;
#1716 = EDGE_CURVE ( 'NONE', #24486, #19788, #12550, .T. ) ;
#1717 = CARTESIAN_POINT ( 'NONE',  ( 4.000000000000003553, -6.690598923241489970, 1.387499999999999956 ) ) ;
#1718 = FACE_OUTER_BOUND ( 'NONE', #4223, .T. ) ;
#1719 = DIRECTION ( 'NONE',  ( -0.7705132427757840352, 0.6374239897486960738, 0.000000000000000000 ) ) ;
#1720 = LINE ( 'NONE', #18068, #3840 ) ;
#1721 = CARTESIAN_POINT ( 'NONE',  ( -2.000000000000000888, -25.76874999877096784, 12.46410161513774817 ) ) ;
#1722 = AXIS2_PLACEMENT_3D ( 'NONE', #7012, #2971, #10938 ) ;
#1723 = CARTESIAN_POINT ( 'NONE',  ( 1.878215178125000939, 27.42812499938548498, 12.25316411605952283 ) ) ;
#1724 = EDGE_CURVE ( 'NONE', #364, #9403, #2359, .T. ) ;
#1725 = CIRCLE ( 'NONE', #17586, 0.5000000000000001110 ) ;
#1726 = CARTESIAN_POINT ( 'NONE',  ( 21.21320343559646915, 21.21320343559638744, 8.999999999999992895 ) ) ;
#1727 = CARTESIAN_POINT ( 'NONE',  ( 3.469446951953614189E-15, 35.50000000000000711, 8.999999999999992895 ) ) ;
#1728 = CARTESIAN_POINT ( 'NONE',  ( 3.834746474454188013E-15, 26.40624999877096357, 4.999999999999992006 ) ) ;
#1729 = VERTEX_POINT ( 'NONE', #20262 ) ;
#1730 = CARTESIAN_POINT ( 'NONE',  ( -2.000000000000003997, -29.12500000000000000, 5.535898384862238508 ) ) ;
#1731 = ORIENTED_EDGE ( 'NONE', *, *, #9338, .T. ) ;
#1732 = AXIS2_PLACEMENT_3D ( 'NONE', #24806, #16316, #18922 ) ;
#1733 = ORIENTED_EDGE ( 'NONE', *, *, #2952, .T. ) ;
#1734 = LINE ( 'NONE', #26, #23734 ) ;
#1735 = ORIENTED_EDGE ( 'NONE', *, *, #14508, .F. ) ;
#1736 = CARTESIAN_POINT ( 'NONE',  ( 3.756430356249996994, -27.72812499938548569, 8.999999999999992895 ) ) ;
#1737 = ORIENTED_EDGE ( 'NONE', *, *, #16361, .T. ) ;
#1738 = ORIENTED_EDGE ( 'NONE', *, *, #1394, .F. ) ;
#1739 = CARTESIAN_POINT ( 'NONE',  ( -3.999999999999996447, 28.82499999999999929, 8.999999999999992895 ) ) ;
#1740 = EDGE_CURVE ( 'NONE', #19049, #20151, #10315, .T. ) ;
#1741 = CIRCLE ( 'NONE', #5077, 5.500000000000000000 ) ;
#1742 = ORIENTED_EDGE ( 'NONE', *, *, #11468, .F. ) ;
#1743 = CARTESIAN_POINT ( 'NONE',  ( 2.000000000000000888, 27.62500000000000000, 12.46410161513774817 ) ) ;
#1744 = DIRECTION ( 'NONE',  ( 0.000000000000000000, 0.000000000000000000, 1.000000000000000000 ) ) ;
#1745 = VECTOR ( 'NONE', #14065, 1000.000000000000000 ) ;
#1746 = VECTOR ( 'NONE', #2061, 1000.000000000000000 ) ;
#1747 = CARTESIAN_POINT ( 'NONE',  ( 3.469446951953614189E-15, -8.999999999999992895, 18.00000000000000000 ) ) ;
#1748 = DIRECTION ( 'NONE',  ( 0.000000000000000000, 0.000000000000000000, -1.000000000000000000 ) ) ;
#1749 = CARTESIAN_POINT ( 'NONE',  ( 21.14697593998939595, 18.49077856202994852, 5.746835883940462963 ) ) ;
#1750 =( BOUNDED_CURVE ( )  B_SPLINE_CURVE ( 2, ( #23869, #8175, #5954, #17730, #23996, #1640, #19806, #25699, #18130 ),
 .UNSPECIFIED., .F., .F. ) 
 B_SPLINE_CURVE_WITH_KNOTS ( ( 3, 2, 2, 2, 3 ),
 ( 0.5250000000000000222, 0.5333333333333333259, 0.5500000000000000444, 0.5666666666666666519, 0.5750000000000000666 ),
 .UNSPECIFIED. ) 
 CURVE ( )  GEOMETRIC_REPRESENTATION_ITEM ( )  RATIONAL_B_SPLINE_CURVE ( ( 0.9330127018922194093, 0.9330127018922194093, 1.000000000000000000, 0.8660254037844387076, 1.000000000000000000, 0.8660254037844387076, 1.000000000000000000, 0.9330127018922189652, 0.9330127018922194093 ) ) 
 REPRESENTATION_ITEM ( '' )  );
#1751 = VECTOR ( 'NONE', #15740, 1000.000000000000000 ) ;
#1752 = CYLINDRICAL_SURFACE ( 'NONE', #20479, 4.000000000000000000 ) ;
#1753 = CARTESIAN_POINT ( 'NONE',  ( 1.071796769724488563, 29.08615380933863648, 4.999999999999988454 ) ) ;
#1754 = CARTESIAN_POINT ( 'NONE',  ( -1.999999999999995781, 28.75000000000000000, 5.535898384862237620 ) ) ;
#1755 =( BOUNDED_SURFACE ( )  B_SPLINE_SURFACE ( 1, 2, ( 
 ( #22911, #15204, #2653, #1193, #9174, #25135, #10614, #9695, #23676, #25264, #1721, #3664, #17416, #19369, #7464, #5253, #9553, #25767, #1338, #21336, #23423, #21471, #7344, #13619, #21717, #1584, #17542, #3801, #9312, #21202, #3418, #17679, #19488, #23558, #25648, #13231, #11395, #17297, #15321, #11518, #25515, #1463, #5639, #5510, #9435, #13500, #7728, #15713, #19235, #7603, #5753, #13740, #15588, #25379, #3545, #15454, #21584, #11642, #19617, #23289, #7847, #11781, #19758, #3280, #11253, #9816, #1855, #17801, #23172, #5374, #13364, #10449, #6409, #24330, #22095, #8243, #8123, #22357, #23805, #14399, #14270, #10068, #17922, #16362, #4441, #12414, #21852, #2101, #20381, #20261, #10314, #19998, #18444, #18069, #2479, #4051, #152, #15832, #23941, #22236, #2238, #275, #2358, #21976, #540, #12020, #3934, #4319, #14005, #5893, #13878, #7988, #16098, #13, #9937, #18308, #11903, #19871, #4184, #15977, #1971 ),
 ( #24062, #12160, #6024, #14129, #6145, #24189, #20136, #10195, #6279, #18191, #12294, #16219, #401, #8370, #4568, #18691, #6532, #17001, #20785, #20527, #22630, #4718, #11101, #12690, #6660, #6924, #2621, #24571, #15036, #24454, #12549, #8754, #23016, #14648, #10582, #16883, #20662, #14784, #24848, #7049, #12813, #2866, #5100, #18577, #14515, #2743, #12942, #4837, #8901, #20922, #16492, #661, #8630, #16608, #13080, #3006, #14909, #21055, #10705, #3134, #16744, #22759, #19078, #6802, #8512, #22879, #779, #24713, #4961, #10835, #10977, #18830, #22486, #919, #18960, #1046, #9018, #24966, #13469, #13202, #15291, #23258, #3766, #5344, #25234, #25481, #21173, #17267, #7698, #17129, #5223, #1433, #15679, #7314, #23144, #9521, #13326, #7431, #19202, #25101, #5724, #3245, #13705, #1298, #7187, #25349, #15175, #11219, #9280, #21436, #21681, #21302, #11360, #25614, #1685, #11744, #3382, #1159, #17503, #11488, #21555 ) ),
 .UNSPECIFIED., .F., .F., .F. ) 
 B_SPLINE_SURFACE_WITH_KNOTS ( ( 2, 2 ),
 ( 3, 2, 2, 2, 2, 2, 2, 2, 2, 2, 2, 2, 2, 2, 2, 2, 2, 2, 2, 2, 2, 2, 2, 2, 2, 2, 2, 2, 2, 2, 2, 2, 2, 2, 2, 2, 2, 2, 2, 2, 2, 2, 2, 2, 2, 2, 2, 2, 2, 2, 2, 2, 2, 2, 2, 2, 2, 2, 2, 2, 3 ),
 ( 0.000000000000000000, 1.000000000000000000 ),
 ( 0.000000000000000000, 0.01666666666666666644, 0.03333333333333333287, 0.05000000000000000278, 0.06666666666666666574, 0.08333333333333332871, 0.1000000000000000056, 0.1166666666666666685, 0.1333333333333333315, 0.1499999999999999944, 0.1666666666666666574, 0.1833333333333333204, 0.2000000000000000111, 0.2166666666666666741, 0.2333333333333333370, 0.2500000000000000000, 0.2666666666666666630, 0.2833333333333333259, 0.2999999999999999889, 0.3166666666666666519, 0.3333333333333333148, 0.3499999999999999778, 0.3666666666666666408, 0.3833333333333333592, 0.4000000000000000222, 0.4166666666666666852, 0.4333333333333333481, 0.4500000000000000111, 0.4666666666666666741, 0.4833333333333333370, 0.5000000000000000000, 0.5166666666666667185, 0.5333333333333333259, 0.5500000000000000444, 0.5666666666666666519, 0.5833333333333333703, 0.5999999999999999778, 0.6166666666666666963, 0.6333333333333333037, 0.6500000000000000222, 0.6666666666666666297, 0.6833333333333333481, 0.6999999999999999556, 0.7166666666666666741, 0.7333333333333332815, 0.7500000000000000000, 0.7666666666666667185, 0.7833333333333333259, 0.8000000000000000444, 0.8166666666666666519, 0.8333333333333333703, 0.8499999999999999778, 0.8666666666666666963, 0.8833333333333333037, 0.9000000000000000222, 0.9166666666666666297, 0.9333333333333333481, 0.9499999999999999556, 0.9666666666666666741, 0.9833333333333332815, 1.000000000000000000 ),
 .UNSPECIFIED. ) 
 GEOMETRIC_REPRESENTATION_ITEM ( )  RATIONAL_B_SPLINE_SURFACE ( (
 ( 1.000000000000000000, 0.8660254037844387076, 1.000000000000000000, 0.8660254037844387076, 1.000000000000000000, 0.8660254037844387076, 1.000000000000000000, 0.8660254037844387076, 1.000000000000000000, 0.8660254037844387076, 1.000000000000000000, 0.8660254037844387076, 1.000000000000000000, 0.8660254037844387076, 1.000000000000000000, 0.8660254037844387076, 1.000000000000000000, 0.8660254037844387076, 1.000000000000000000, 0.8660254037844387076, 1.000000000000000000, 0.8660254037844387076, 1.000000000000000000, 0.8660254037844387076, 1.000000000000000000, 0.8660254037844387076, 1.000000000000000000, 0.8660254037844387076, 1.000000000000000000, 0.8660254037844387076, 1.000000000000000000, 0.8660254037844387076, 1.000000000000000000, 0.8660254037844387076, 1.000000000000000000, 0.8660254037844387076, 1.000000000000000000, 0.8660254037844387076, 1.000000000000000000, 0.8660254037844387076, 1.000000000000000000, 0.8660254037844387076, 1.000000000000000000, 0.8660254037844387076, 1.000000000000000000, 0.8660254037844387076, 1.000000000000000000, 0.8660254037844387076, 1.000000000000000000, 0.8660254037844387076, 1.000000000000000000, 0.8660254037844387076, 1.000000000000000000, 0.8660254037844387076, 1.000000000000000000, 0.8660254037844387076, 1.000000000000000000, 0.8660254037844387076, 1.000000000000000000, 0.8660254037844387076, 1.000000000000000000, 0.8660254037844387076, 1.000000000000000000, 0.8660254037844387076, 1.000000000000000000, 0.8660254037844387076, 1.000000000000000000, 0.8660254037844387076, 1.000000000000000000, 0.8660254037844387076, 1.000000000000000000, 0.8660254037844387076, 1.000000000000000000, 0.8660254037844387076, 1.000000000000000000, 0.8660254037844387076, 1.000000000000000000, 0.8660254037844387076, 1.000000000000000000, 0.8660254037844387076, 1.000000000000000000, 0.8660254037844387076, 1.000000000000000000, 0.8660254037844387076, 1.000000000000000000, 0.8660254037844387076, 1.000000000000000000, 0.8660254037844387076, 1.000000000000000000, 0.8660254037844387076, 1.000000000000000000, 0.8660254037844387076, 1.000000000000000000, 0.8660254037844387076, 1.000000000000000000, 0.8660254037844387076, 1.000000000000000000, 0.8660254037844387076, 1.000000000000000000, 0.8660254037844387076, 1.000000000000000000, 0.8660254037844387076, 1.000000000000000000, 0.8660254037844387076, 1.000000000000000000, 0.8660254037844387076, 1.000000000000000000, 0.8660254037844387076, 1.000000000000000000, 0.8660254037844387076, 1.000000000000000000, 0.8660254037844387076, 1.000000000000000000, 0.8660254037844387076, 1.000000000000000000, 0.8660254037844387076, 1.000000000000000000, 0.8660254037844387076, 1.000000000000000000, 0.8660254037844387076, 1.000000000000000000),
 ( 1.000000000000000000, 0.8660254037844387076, 1.000000000000000000, 0.8660254037844387076, 1.000000000000000000, 0.8660254037844387076, 1.000000000000000000, 0.8660254037844387076, 1.000000000000000000, 0.8660254037844387076, 1.000000000000000000, 0.8660254037844387076, 1.000000000000000000, 0.8660254037844387076, 1.000000000000000000, 0.8660254037844387076, 1.000000000000000000, 0.8660254037844387076, 1.000000000000000000, 0.8660254037844387076, 1.000000000000000000, 0.8660254037844387076, 1.000000000000000000, 0.8660254037844387076, 1.000000000000000000, 0.8660254037844387076, 1.000000000000000000, 0.8660254037844387076, 1.000000000000000000, 0.8660254037844387076, 1.000000000000000000, 0.8660254037844387076, 1.000000000000000000, 0.8660254037844387076, 1.000000000000000000, 0.8660254037844387076, 1.000000000000000000, 0.8660254037844387076, 1.000000000000000000, 0.8660254037844387076, 1.000000000000000000, 0.8660254037844387076, 1.000000000000000000, 0.8660254037844387076, 1.000000000000000000, 0.8660254037844387076, 1.000000000000000000, 0.8660254037844387076, 1.000000000000000000, 0.8660254037844387076, 1.000000000000000000, 0.8660254037844387076, 1.000000000000000000, 0.8660254037844387076, 1.000000000000000000, 0.8660254037844387076, 1.000000000000000000, 0.8660254037844387076, 1.000000000000000000, 0.8660254037844387076, 1.000000000000000000, 0.8660254037844387076, 1.000000000000000000, 0.8660254037844387076, 1.000000000000000000, 0.8660254037844387076, 1.000000000000000000, 0.8660254037844387076, 1.000000000000000000, 0.8660254037844387076, 1.000000000000000000, 0.8660254037844387076, 1.000000000000000000, 0.8660254037844387076, 1.000000000000000000, 0.8660254037844387076, 1.000000000000000000, 0.8660254037844387076, 1.000000000000000000, 0.8660254037844387076, 1.000000000000000000, 0.8660254037844387076, 1.000000000000000000, 0.8660254037844387076, 1.000000000000000000, 0.8660254037844387076, 1.000000000000000000, 0.8660254037844387076, 1.000000000000000000, 0.8660254037844387076, 1.000000000000000000, 0.8660254037844387076, 1.000000000000000000, 0.8660254037844387076, 1.000000000000000000, 0.8660254037844387076, 1.000000000000000000, 0.8660254037844387076, 1.000000000000000000, 0.8660254037844387076, 1.000000000000000000, 0.8660254037844387076, 1.000000000000000000, 0.8660254037844387076, 1.000000000000000000, 0.8660254037844387076, 1.000000000000000000, 0.8660254037844387076, 1.000000000000000000, 0.8660254037844387076, 1.000000000000000000, 0.8660254037844387076, 1.000000000000000000, 0.8660254037844387076, 1.000000000000000000, 0.8660254037844387076, 1.000000000000000000, 0.8660254037844387076, 1.000000000000000000, 0.8660254037844387076, 1.000000000000000000) ) ) 
 REPRESENTATION_ITEM ( '' )  SURFACE ( )  );
#1756 = CARTESIAN_POINT ( 'NONE',  ( -1.878215178124995832, -5.746835883940462963, 0.4031249993854852942 ) ) ;
#1757 = CARTESIAN_POINT ( 'NONE',  ( 18.22334004483017011, 23.53573480074883761, 8.999999999999992895 ) ) ;
#1758 = CARTESIAN_POINT ( 'NONE',  ( 1.057460391440397258E-14, -29.55624999877096926, 4.999999999999992006 ) ) ;
#1759 = CIRCLE ( 'NONE', #16381, 0.5000000000000002220 ) ;
#1760 = ORIENTED_EDGE ( 'NONE', *, *, #15178, .F. ) ;
#1761 = ORIENTED_EDGE ( 'NONE', *, *, #2756, .F. ) ;
#1762 = CARTESIAN_POINT ( 'NONE',  ( 3.756430356250004543, 25.74062499938548498, 6.831223922626973533 ) ) ;
#1763 = ADVANCED_FACE ( 'NONE', ( #402 ), #8371, .F. ) ;
#1764 = VECTOR ( 'NONE', #1067, 1000.000000000000000 ) ;
#1765 = EDGE_LOOP ( 'NONE', ( #24272, #20790, #5968, #16322 ) ) ;
#1766 = CARTESIAN_POINT ( 'NONE',  ( -26.25859848311282363, -16.66421332384654974, -6.500000000000000000 ) ) ;
#1767 = CARTESIAN_POINT ( 'NONE',  ( 3.756430356250004099, 29.34062499938548640, 6.831223922626973533 ) ) ;
#1768 = CARTESIAN_POINT ( 'NONE',  ( 16.36952198446861217, 19.19794910921473630, 5.535898384862237620 ) ) ;
#1769 = ORIENTED_EDGE ( 'NONE', *, *, #24964, .F. ) ;
#1770 = VERTEX_POINT ( 'NONE', #6410 ) ;
#1771 = VECTOR ( 'NONE', #22592, 1000.000000000000000 ) ;
#1772 = CARTESIAN_POINT ( 'NONE',  ( -4.000000000000057732, -6.690598923241522833, 4.237499999999998934 ) ) ;
#1773 = EDGE_LOOP ( 'NONE', ( #24159, #22801, #5797, #22926 ) ) ;
#1774 = CYLINDRICAL_SURFACE ( 'NONE', #5980, 31.10000000000000142 ) ;
#1775 = CARTESIAN_POINT ( 'NONE',  ( 0.000000000000000000, 0.000000000000000000, -6.500000000000000000 ) ) ;
#1776 = CARTESIAN_POINT ( 'NONE',  ( 1.878215178125006934, 27.91562499938549280, 5.746835883940462963 ) ) ;
#1777 = DIRECTION ( 'NONE',  ( 0.000000000000000000, 0.000000000000000000, 1.000000000000000000 ) ) ;
#1778 = CARTESIAN_POINT ( 'NONE',  ( 2.000000000000000000, 27.62500000000000355, 12.46410161513774817 ) ) ;
#1779 = AXIS2_PLACEMENT_3D ( 'NONE', #11090, #1544, #9511 ) ;
#1780 = AXIS2_PLACEMENT_3D ( 'NONE', #1681, #25346, #11485 ) ;
#1781 = DIRECTION ( 'NONE',  ( 0.8090169943749474513, -0.5877852522924730261, 0.000000000000000000 ) ) ;
#1782 = DIRECTION ( 'NONE',  ( -0.4257792915650642218, 0.9048270524660235736, 0.000000000000000000 ) ) ;
#1783 = CARTESIAN_POINT ( 'NONE',  ( 0.000000000000000000, 0.000000000000000000, -6.500000000000000000 ) ) ;
#1784 = DIRECTION ( 'NONE',  ( 1.000000000000000000, 0.000000000000000000, 0.000000000000000000 ) ) ;
#1785 = CARTESIAN_POINT ( 'NONE',  ( 15.98945208958084230, 21.64630633907315982, 11.30940107675849404 ) ) ;
#1786 = CARTESIAN_POINT ( 'NONE',  ( 20.79998790990604718, 20.79998790990596902, 4.662447845253954171 ) ) ;
#1787 = CARTESIAN_POINT ( 'NONE',  ( -2.451530025009351910, -31.00322564728512020, -2.750000000000000000 ) ) ;
#1788 = DIRECTION ( 'NONE',  ( 1.000000000000000000, 0.000000000000000000, 0.000000000000000000 ) ) ;
#1789 = EDGE_CURVE ( 'NONE', #2251, #13124, #15580, .T. ) ;
#1790 = CYLINDRICAL_SURFACE ( 'NONE', #9593, 31.10000000000000142 ) ;
#1791 = CARTESIAN_POINT ( 'NONE',  ( 20.20656826142283435, 23.64116323484230975, -6.500000000000000000 ) ) ;
#1792 = ORIENTED_EDGE ( 'NONE', *, *, #11977, .T. ) ;
#1793 = CARTESIAN_POINT ( 'NONE',  ( -1.999999999999995781, 25.99374999877096926, 5.535898384862237620 ) ) ;
#1794 = CARTESIAN_POINT ( 'NONE',  ( 3.999999999999996447, -27.02500000000000213, 8.999999999999992895 ) ) ;
#1796 = VERTEX_POINT ( 'NONE', #541 ) ;
#1795 = DIRECTION ( 'NONE',  ( -0.9980267284282718920, -0.06279051952930848890, 0.000000000000000000 ) ) ;
#1797 = CARTESIAN_POINT ( 'NONE',  ( 2.672651547586948120E-15, 27.84062499938548640, 13.33755215474603162 ) ) ;
#1798 = EDGE_CURVE ( 'NONE', #14524, #18045, #15690, .T. ) ;
#1799 = CARTESIAN_POINT ( 'NONE',  ( 3.959305671612554781E-15, 30.00000000000000355, 12.99999999999999289 ) ) ;
#1800 = CARTESIAN_POINT ( 'NONE',  ( 11.52193136556786257, 23.36965697125208052, 20.00001200000000168 ) ) ;
#1801 = CARTESIAN_POINT ( 'NONE',  ( 4.000000000000003553, 26.33124999877097139, 6.690598923241489970 ) ) ;
#1802 = ORIENTED_EDGE ( 'NONE', *, *, #22163, .T. ) ;
#1803 = ORIENTED_EDGE ( 'NONE', *, *, #15696, .F. ) ;
#1804 = EDGE_CURVE ( 'NONE', #17932, #25409, #2835, .T. ) ;
#1805 = FILL_AREA_STYLE_COLOUR ( '', #19762 ) ;
#1806 = CARTESIAN_POINT ( 'NONE',  ( 1.878215178125003382, 25.66562499938548214, 5.746835883940462963 ) ) ;
#1807 = AXIS2_PLACEMENT_3D ( 'NONE', #12216, #16416, #18236 ) ;
#1808 = CARTESIAN_POINT ( 'NONE',  ( 1.878215178125004048, -5.746835883940462963, 2.915624999385482585 ) ) ;
#1809 = EDGE_CURVE ( 'NONE', #2418, #22249, #8902, .T. ) ;
#1810 = CIRCLE ( 'NONE', #2223, 0.5000000000000007772 ) ;
#1811 = CARTESIAN_POINT ( 'NONE',  ( -1.057460391440397258E-14, 29.10624999877096641, 4.999999999999992006 ) ) ;
#1812 =( NAMED_UNIT ( * ) PLANE_ANGLE_UNIT ( ) SI_UNIT ( $, .RADIAN. ) );
#1813 = CARTESIAN_POINT ( 'NONE',  ( -18.28012134629613783, -25.16042852506070560, 1.000000000000000000 ) ) ;
#1814 = DIRECTION ( 'NONE',  ( 1.000000000000000000, 0.000000000000000000, 0.000000000000000000 ) ) ;
#1815 = LINE ( 'NONE', #22055, #16365 ) ;
#1816 = DIRECTION ( 'NONE',  ( 0.000000000000000000, 1.000000000000000000, -0.000000000000000000 ) ) ;
#1817 = CARTESIAN_POINT ( 'NONE',  ( -3.999999999999995559, 26.93124999877096926, 6.690598923241487306 ) ) ;
#1818 = CARTESIAN_POINT ( 'NONE',  ( 18.01575495898401513, 18.01575495898394408, 13.33755215474602984 ) ) ;
#1819 = CARTESIAN_POINT ( 'NONE',  ( 16.21484237521500305, 21.87169662470731524, 6.690598923241487306 ) ) ;
#1820 = ORIENTED_EDGE ( 'NONE', *, *, #932, .T. ) ;
#1821 = CARTESIAN_POINT ( 'NONE',  ( -1.859271017917182139E-15, -29.78124999877096712, 12.99999999999999289 ) ) ;
#1822 = CARTESIAN_POINT ( 'NONE',  ( 0.000000000000000000, 0.000000000000000000, -6.500000000000000000 ) ) ;
#1823 = CARTESIAN_POINT ( 'NONE',  ( -1.878215178124998497, 27.35312499938548569, 12.25316411605951927 ) ) ;
#1824 = CARTESIAN_POINT ( 'NONE',  ( -30.91344420362543843, 3.401318489841417048, -2.750000000000000000 ) ) ;
#1825 = STYLED_ITEM ( 'NONE', ( #22348 ), #7868 ) ;
#1826 = CARTESIAN_POINT ( 'NONE',  ( -1.071796769724485676, 26.21740381056767077, 12.99999999999999467 ) ) ;
#1827 = CARTESIAN_POINT ( 'NONE',  ( 0.000000000000000000, 0.000000000000000000, 1.000000000000000000 ) ) ;
#1828 = ORIENTED_EDGE ( 'NONE', *, *, #6632, .F. ) ;
#1829 = CARTESIAN_POINT ( 'NONE',  ( 3.834746474454188013E-15, 27.36250000000000426, 4.999999999999992006 ) ) ;
#1830 = LINE ( 'NONE', #7575, #21316 ) ;
#1832 = ORIENTED_EDGE ( 'NONE', *, *, #6525, .F. ) ;
#1831 = DIRECTION ( 'NONE',  ( -0.6374239897486843054, 0.7705132427757935831, 0.000000000000000000 ) ) ;
#1833 = AXIS2_PLACEMENT_3D ( 'NONE', #14255, #20249, #2087 ) ;
#1834 = ORIENTED_EDGE ( 'NONE', *, *, #13308, .F. ) ;
#1835 = EDGE_CURVE ( 'NONE', #3169, #383, #19018, .T. ) ;
#1836 = ORIENTED_EDGE ( 'NONE', *, *, #17614, .T. ) ;
#1837 = ORIENTED_EDGE ( 'NONE', *, *, #14330, .T. ) ;
#1838 = ORIENTED_EDGE ( 'NONE', *, *, #4123, .F. ) ;
#1839 = EDGE_CURVE ( 'NONE', #12074, #6033, #921, .T. ) ;
#1840 = CARTESIAN_POINT ( 'NONE',  ( 30.54913349766223973, 5.827558883615938434, 1.000000000000000000 ) ) ;
#1841 = DIRECTION ( 'NONE',  ( 1.000000000000000000, 0.000000000000000000, 0.000000000000000000 ) ) ;
#1842 = EDGE_CURVE ( 'NONE', #7738, #14582, #13104, .T. ) ;
#1843 = CARTESIAN_POINT ( 'NONE',  ( 1.878215178125003382, 27.01562499938548711, 5.746835883940462963 ) ) ;
#1844 = EDGE_CURVE ( 'NONE', #23396, #4202, #5165, .T. ) ;
#1845 = CARTESIAN_POINT ( 'NONE',  ( -3.756430356249995661, -6.831223922626973533, 3.478124999385480809 ) ) ;
#1846 = CARTESIAN_POINT ( 'NONE',  ( 3.735045420075836212E-15, -4.662447845253954171, 0.8156249993854834957 ) ) ;
#1847 =( LENGTH_UNIT ( ) NAMED_UNIT ( * ) SI_UNIT ( .MILLI., .METRE. ) );
#1848 = CARTESIAN_POINT ( 'NONE',  ( 3.756430356250003655, 28.40312499938548640, 8.999999999999992895 ) ) ;
#1849 = CARTESIAN_POINT ( 'NONE',  ( -1.057460391440397258E-14, 28.71250000000000213, 4.999999999999992006 ) ) ;
#1850 = DIRECTION ( 'NONE',  ( 1.000000000000000000, 0.000000000000000000, 0.000000000000000000 ) ) ;
#1851 = CARTESIAN_POINT ( 'NONE',  ( 3.752267015613588906E-15, -4.381197846482986158, 2.362499999999997602 ) ) ;
#1852 = DIRECTION ( 'NONE',  ( 1.000000000000000000, 0.000000000000000000, 0.000000000000000000 ) ) ;
#1853 = CARTESIAN_POINT ( 'NONE',  ( -0.5000000000000000000, 6.000000000000000000, 20.00000000000000000 ) ) ;
#1854 = LINE ( 'NONE', #9815, #15968 ) ;
#1855 = CARTESIAN_POINT ( 'NONE',  ( 3.999999999999996447, -27.86874999877096570, 8.999999999999992895 ) ) ;
#1856 = CARTESIAN_POINT ( 'NONE',  ( 2.672651547586948120E-15, 26.94062499938548783, 13.33755215474602984 ) ) ;
#1857 = CARTESIAN_POINT ( 'NONE',  ( 1.626862140677534194E-14, 27.58750000000000213, 12.99999999999999289 ) ) ;
#1858 = DIRECTION ( 'NONE',  ( 0.000000000000000000, 0.000000000000000000, 1.000000000000000000 ) ) ;
#1859 = CARTESIAN_POINT ( 'NONE',  ( 1.999999999999998224, -26.14374999877096784, 12.46410161513774639 ) ) ;
#1860 = ORIENTED_EDGE ( 'NONE', *, *, #20590, .T. ) ;
#1861 = DIRECTION ( 'NONE',  ( 0.000000000000000000, 0.000000000000000000, -1.000000000000000000 ) ) ;
#1862 = ORIENTED_EDGE ( 'NONE', *, *, #1367, .F. ) ;
#1863 = ORIENTED_EDGE ( 'NONE', *, *, #5533, .F. ) ;
#1864 = DIRECTION ( 'NONE',  ( 1.000000000000000000, 0.000000000000000000, 0.000000000000000000 ) ) ;
#1865 =( BOUNDED_CURVE ( )  B_SPLINE_CURVE ( 2, ( #8288, #10502, #16271, #24241, #8427, #24382, #6458, #706, #14446 ),
 .UNSPECIFIED., .F., .F. ) 
 B_SPLINE_CURVE_WITH_KNOTS ( ( 3, 2, 2, 2, 3 ),
 ( 0.6750000000000000444, 0.6833333333333333481, 0.6999999999999999556, 0.7166666666666666741, 0.7249999999999999778 ),
 .UNSPECIFIED. ) 
 CURVE ( )  GEOMETRIC_REPRESENTATION_ITEM ( )  RATIONAL_B_SPLINE_CURVE ( ( 0.9330127018922194093, 0.9330127018922198534, 1.000000000000000000, 0.8660254037844387076, 1.000000000000000000, 0.8660254037844387076, 1.000000000000000000, 0.9330127018922194093, 0.9330127018922194093 ) ) 
 REPRESENTATION_ITEM ( '' )  );
#1866 = ORIENTED_EDGE ( 'NONE', *, *, #3698, .F. ) ;
#1867 = CARTESIAN_POINT ( 'NONE',  ( -3.756430356250003655, -27.95312499938548711, 8.999999999999992895 ) ) ;
#1868 = ORIENTED_EDGE ( 'NONE', *, *, #2700, .T. ) ;
#1869 = CARTESIAN_POINT ( 'NONE',  ( 3.369928719974892281E-15, 25.50624999877096855, 4.999999999999992006 ) ) ;
#1870 = EDGE_CURVE ( 'NONE', #14796, #13703, #23548, .T. ) ;
#1871 = ORIENTED_EDGE ( 'NONE', *, *, #10098, .F. ) ;
#1872 = CARTESIAN_POINT ( 'NONE',  ( 4.000000000000003553, 26.80000000000000071, 8.999999999999992895 ) ) ;
#1873 = DIRECTION ( 'NONE',  ( 0.000000000000000000, 0.000000000000000000, 1.000000000000000000 ) ) ;
#1874 = ADVANCED_FACE ( 'NONE', ( #24967 ), #378, .T. ) ;
#1875 = CARTESIAN_POINT ( 'NONE',  ( 3.735045420075836212E-15, -4.662447845253954171, 0.3656249993854837066 ) ) ;
#1876 = CARTESIAN_POINT ( 'NONE',  ( -30.12293631110050995, -7.734255490826679846, -6.500000000000000000 ) ) ;
#1877 = CARTESIAN_POINT ( 'NONE',  ( 23.05843772344798381, 17.74604296752915999, 8.999999999999992895 ) ) ;
#1878 = DIRECTION ( 'NONE',  ( 0.000000000000000000, 0.000000000000000000, 1.000000000000000000 ) ) ;
#1879 = CARTESIAN_POINT ( 'NONE',  ( 5.112995299272250684E-15, 25.56250000000000711, 4.999999999999992006 ) ) ;
#1880 = APPLICATION_PROTOCOL_DEFINITION ( 'draft international standard', 'automotive_design', 1998, #20643 ) ;
#1881 = CARTESIAN_POINT ( 'NONE',  ( 3.752267015613588906E-15, 29.16250000000000142, 4.381197846482986158 ) ) ;
#1882 = DIRECTION ( 'NONE',  ( -0.000000000000000000, -1.000000000000000000, -0.000000000000000000 ) ) ;
#1883 = CARTESIAN_POINT ( 'NONE',  ( 20.48178985837210320, 20.48178985837202504, 4.662447845253954171 ) ) ;
#1884 = DIRECTION ( 'NONE',  ( 0.000000000000000000, 0.000000000000000000, 1.000000000000000000 ) ) ;
#1885 = ORIENTED_EDGE ( 'NONE', *, *, #23874, .T. ) ;
#1886 = EDGE_LOOP ( 'NONE', ( #10348, #2305, #20236, #25362 ) ) ;
#1887 = CARTESIAN_POINT ( 'NONE',  ( 4.000000000000000888, 29.85624999877096997, 11.30940107675849760 ) ) ;
#1888 = ORIENTED_EDGE ( 'NONE', *, *, #24958, .F. ) ;
#1889 = DIRECTION ( 'NONE',  ( -0.1253332335643051187, -0.9921147013144777649, 0.000000000000000000 ) ) ;
#1890 = CARTESIAN_POINT ( 'NONE',  ( -3.756430356249996994, 26.82812499938548711, 8.999999999999992895 ) ) ;
#1891 = CARTESIAN_POINT ( 'NONE',  ( 0.000000000000000000, 0.000000000000000000, -6.500000000000000000 ) ) ;
#1892 = FACE_OUTER_BOUND ( 'NONE', #19692, .T. ) ;
#1893 = ORIENTED_EDGE ( 'NONE', *, *, #23260, .F. ) ;
#1894 = VERTEX_POINT ( 'NONE', #17356 ) ;
#1895 = CARTESIAN_POINT ( 'NONE',  ( 9.296355089585910693E-16, 26.18124999877096926, 12.99999999999999289 ) ) ;
#1896 = EDGE_LOOP ( 'NONE', ( #5864, #2010, #1837, #5903 ) ) ;
#1897 = FACE_OUTER_BOUND ( 'NONE', #3841, .T. ) ;
#1898 = EDGE_CURVE ( 'NONE', #6457, #14723, #11710, .T. ) ;
#1899 =( BOUNDED_CURVE ( )  B_SPLINE_CURVE ( 2, ( #11750, #22065, #19966, #5728, #7956, #19729, #4154, #1826, #8094 ),
 .UNSPECIFIED., .F., .F. ) 
 B_SPLINE_CURVE_WITH_KNOTS ( ( 3, 2, 2, 2, 3 ),
 ( 0.2250000000000000056, 0.2333333333333333370, 0.2500000000000000000, 0.2666666666666666630, 0.2750000000000000222 ),
 .UNSPECIFIED. ) 
 CURVE ( )  GEOMETRIC_REPRESENTATION_ITEM ( )  RATIONAL_B_SPLINE_CURVE ( ( 0.9330127018922194093, 0.9330127018922194093, 1.000000000000000000, 0.8660254037844387076, 1.000000000000000000, 0.8660254037844387076, 1.000000000000000000, 0.9330127018922191873, 0.9330127018922194093 ) ) 
 REPRESENTATION_ITEM ( '' )  );
#1900 = CYLINDRICAL_SURFACE ( 'NONE', #11777, 4.000000000000000000 ) ;
#1901 = CARTESIAN_POINT ( 'NONE',  ( 3.756430356250004987, 27.84062499938548640, 8.999999999999992895 ) ) ;
#1902 = CARTESIAN_POINT ( 'NONE',  ( 2.006336132164985451E-12, 39.00000000001113420, 3.500000000010202061 ) ) ;
#1903 = CARTESIAN_POINT ( 'NONE',  ( 2.000000000000003553, 27.32500000000000995, 5.535898384862238508 ) ) ;
#1904 =( BOUNDED_CURVE ( )  B_SPLINE_CURVE ( 2, ( #10676, #20494, #20632, #22333, #12389, #4415, #20108 ),
 .UNSPECIFIED., .F., .F. ) 
 B_SPLINE_CURVE_WITH_KNOTS ( ( 3, 2, 2, 3 ),
 ( 0.2500000000000002776, 0.2666666666666669405, 0.2833333333333335480, 0.3000000000000002109 ),
 .UNSPECIFIED. ) 
 CURVE ( )  GEOMETRIC_REPRESENTATION_ITEM ( )  RATIONAL_B_SPLINE_CURVE ( ( 0.9999999999999977796, 0.8660254037844409281, 1.000000000000000000, 0.8660254037844387076, 1.000000000000000000, 0.8660254037844369313, 1.000000000000001776 ) ) 
 REPRESENTATION_ITEM ( '' )  );
#1905 = ADVANCED_FACE ( 'NONE', ( #13943 ), #13433, .F. ) ;
#1906 = CARTESIAN_POINT ( 'NONE',  ( 1.878215178125000939, 25.96562499938548285, 12.25316411605952283 ) ) ;
#1907 = EDGE_CURVE ( 'NONE', #10879, #16189, #17053, .T. ) ;
#1908 = CYLINDRICAL_SURFACE ( 'NONE', #70, 31.10000000000000142 ) ;
#1909 = CIRCLE ( 'NONE', #25701, 31.10000000000000142 ) ;
#1910 = DIRECTION ( 'NONE',  ( 0.8660254037844397068, 0.4999999999999983347, 0.000000000000000000 ) ) ;
#1911 = CARTESIAN_POINT ( 'NONE',  ( 21.75237235625120036, 16.09551810675874961, 11.30940107675849760 ) ) ;
#1912 = CARTESIAN_POINT ( 'NONE',  ( 17.93165849759071762, 23.24405325350938867, 11.16877607737301226 ) ) ;
#1913 = CARTESIAN_POINT ( 'NONE',  ( -1.071796769724498999, -28.45134618820330275, 12.99999999999998757 ) ) ;
#1914 = CARTESIAN_POINT ( 'NONE',  ( -1.878215178125004048, -26.11562499938548498, 5.746835883940462963 ) ) ;
#1915 = CARTESIAN_POINT ( 'NONE',  ( 23.58876780933789519, 18.27637305341907492, 11.16877607737301403 ) ) ;
#1916 = CARTESIAN_POINT ( 'NONE',  ( 4.648177544792954952E-15, 25.73124999877097707, 12.99999999999999289 ) ) ;
#1917 = EDGE_LOOP ( 'NONE', ( #11967, #217, #10984, #17041 ) ) ;
#1918 = CARTESIAN_POINT ( 'NONE',  ( -1.999999999999998224, 28.39374999877096784, 12.46410161513774639 ) ) ;
#1919 = CARTESIAN_POINT ( 'NONE',  ( 1.999999999999998224, -26.64999999999999858, 12.46410161513774639 ) ) ;
#1921 = ORIENTED_EDGE ( 'NONE', *, *, #17399, .T. ) ;
#1920 = CARTESIAN_POINT ( 'NONE',  ( 8.217531866530997320, -29.99470236596036088, 1.000000000000000000 ) ) ;
#1922 = CARTESIAN_POINT ( 'NONE',  ( 2.672651547586948120E-15, 28.74062499938548854, 13.33755215474603162 ) ) ;
#1923 = CARTESIAN_POINT ( 'NONE',  ( -1.859271017917182139E-15, -29.78124999877096712, 12.99999999999999289 ) ) ;
#1924 = CARTESIAN_POINT ( 'NONE',  ( 15.85973458909325728, 20.67279826512042362, 20.00001200000000168 ) ) ;
#1925 = CARTESIAN_POINT ( 'NONE',  ( 4.000000000000001776, 26.25624999877096855, 11.30940107675849760 ) ) ;
#1926 = VERTEX_POINT ( 'NONE', #1520 ) ;
#1927 = VERTEX_POINT ( 'NONE', #21404 ) ;
#1928 = CARTESIAN_POINT ( 'NONE',  ( 3.756430356250002323, 26.45312499938549067, 11.16877607737301226 ) ) ;
#1929 = CARTESIAN_POINT ( 'NONE',  ( 3.756430356250003211, -6.831223922626973533, 4.228124999385484806 ) ) ;
#1930 = ADVANCED_FACE ( 'NONE', ( #3868 ), #25442, .F. ) ;
#1931 = PLANE ( 'NONE',  #2503 ) ;
#1932 = CARTESIAN_POINT ( 'NONE',  ( -4.000000000000012434, -11.30940107675848516, 3.862499999999996714 ) ) ;
#1933 = EDGE_CURVE ( 'NONE', #14528, #5581, #19396, .T. ) ;
#1934 = CARTESIAN_POINT ( 'NONE',  ( 19.83756213693951764, 21.35331166479149090, 4.999999999999995559 ) ) ;
#1935 = CARTESIAN_POINT ( 'NONE',  ( 19.96119519019960720, 18.44544566234749183, 12.99999999999999112 ) ) ;
#1936 = LINE ( 'NONE', #24027, #12005 ) ;
#1937 = DIRECTION ( 'NONE',  ( 0.000000000000000000, 1.000000000000000000, 0.000000000000000000 ) ) ;
#1938 = CARTESIAN_POINT ( 'NONE',  ( 15.62472262396960154, 20.93711737988828503, 11.16877607737301226 ) ) ;
#1939 = FACE_OUTER_BOUND ( 'NONE', #16075, .T. ) ;
#1940 = VERTEX_POINT ( 'NONE', #13557 ) ;
#1941 = CARTESIAN_POINT ( 'NONE',  ( -5.618699665603582361, 38.72260848564139479, 10.34687723573376594 ) ) ;
#1942 = CARTESIAN_POINT ( 'NONE',  ( 5.501714610360307844, 38.82806989278485332, 7.617651621319569522 ) ) ;
#1943 = CARTESIAN_POINT ( 'NONE',  ( 3.756430356250004099, 26.64062499938549067, 6.831223922626973533 ) ) ;
#1944 = DIRECTION ( 'NONE',  ( 1.000000000000000000, 0.000000000000000000, 0.000000000000000000 ) ) ;
#1945 = DIRECTION ( 'NONE',  ( 0.000000000000000000, 0.000000000000000000, -1.000000000000000000 ) ) ;
#1946 = DIRECTION ( 'NONE',  ( 1.000000000000000000, 0.000000000000000000, 0.000000000000000000 ) ) ;
#1947 = ORIENTED_EDGE ( 'NONE', *, *, #3452, .F. ) ;
#1948 = CARTESIAN_POINT ( 'NONE',  ( 1.859271017917182139E-15, 27.08124999877096784, 12.99999999999999289 ) ) ;
#1949 = DIRECTION ( 'NONE',  ( -0.000000000000000000, -1.000000000000000000, -0.000000000000000000 ) ) ;
#1951 = VERTEX_POINT ( 'NONE', #5960 ) ;
#1950 = CARTESIAN_POINT ( 'NONE',  ( 1.071796769724497222, 28.63615380933864429, 4.999999999999992895 ) ) ;
#1952 = ORIENTED_EDGE ( 'NONE', *, *, #14569, .F. ) ;
#1953 = ORIENTED_EDGE ( 'NONE', *, *, #17459, .F. ) ;
#1954 = ORIENTED_EDGE ( 'NONE', *, *, #4739, .T. ) ;
#1955 = LINE ( 'NONE', #10052, #15962 ) ;
#1956 = CARTESIAN_POINT ( 'NONE',  ( -4.000000000000003553, -28.09374999877097068, 8.999999999999992895 ) ) ;
#1957 = DIRECTION ( 'NONE',  ( 0.6845471059286901694, -0.7289686274214101092, 0.000000000000000000 ) ) ;
#1958 = ADVANCED_FACE ( 'NONE', ( #21523 ), #11575, .T. ) ;
#1959 = CARTESIAN_POINT ( 'NONE',  ( 8.012344526598182026E-15, 27.05312499938548854, 4.662447845253954171 ) ) ;
#1960 = CARTESIAN_POINT ( 'NONE',  ( 3.756430356250004099, -6.831223922626973533, 3.778124999385480631 ) ) ;
#1961 = CARTESIAN_POINT ( 'NONE',  ( 2.000000000000000888, -12.46410161513774817, 3.468749998770968901 ) ) ;
#1962 = SURFACE_SIDE_STYLE ('',( #8501 ) ) ;
#1963 = CARTESIAN_POINT ( 'NONE',  ( 3.756430356250003655, 27.95312499938548711, 8.999999999999992895 ) ) ;
#1964 = EDGE_CURVE ( 'NONE', #12794, #16109, #10013, .T. ) ;
#1965 = CARTESIAN_POINT ( 'NONE',  ( 19.66640735175089105, 19.66640735175081289, 4.999999999999992006 ) ) ;
#1966 = DIRECTION ( 'NONE',  ( 0.000000000000000000, -1.000000000000000000, 0.000000000000000000 ) ) ;
#1967 = CARTESIAN_POINT ( 'NONE',  ( 4.000000000000003553, -8.999999999999992895, 1.350000000000000533 ) ) ;
#1968 = DIRECTION ( 'NONE',  ( 0.000000000000000000, -0.000000000000000000, 1.000000000000000000 ) ) ;
#1969 = CARTESIAN_POINT ( 'NONE',  ( 1.071796769724496334, 27.79240381056767362, 4.999999999999992895 ) ) ;
#1970 = EDGE_CURVE ( 'NONE', #13143, #2042, #5277, .T. ) ;
#1971 = CARTESIAN_POINT ( 'NONE',  ( -4.000000000000003553, -29.89374999877096784, 8.999999999999992895 ) ) ;
#1972 = CARTESIAN_POINT ( 'NONE',  ( 3.735045420075836212E-15, 27.16562499938548569, 4.662447845253954171 ) ) ;
#1973 = CARTESIAN_POINT ( 'NONE',  ( 1.071796769724487230, -26.03259618943233278, 4.999999999999992006 ) ) ;
#1974 = DIRECTION ( 'NONE',  ( -0.7071067811865487940, -0.7071067811865463515, 0.000000000000000000 ) ) ;
#1975 = DIRECTION ( 'NONE',  ( 1.000000000000000000, 0.000000000000000000, 0.000000000000000000 ) ) ;
#1976 = ORIENTED_EDGE ( 'NONE', *, *, #13413, .F. ) ;
#1977 = ADVANCED_FACE ( 'NONE', ( #4376 ), #4639, .F. ) ;
#1978 = CARTESIAN_POINT ( 'NONE',  ( 4.000000000000003553, -8.999999999999992895, 4.696874999385483918 ) ) ;
#1980 = EDGE_LOOP ( 'NONE', ( #9772, #7853, #12703, #18590 ) ) ;
#1979 = CARTESIAN_POINT ( 'NONE',  ( 1.626862140677534194E-14, 28.03750000000000497, 12.99999999999999289 ) ) ;
#1981 = ORIENTED_EDGE ( 'NONE', *, *, #20383, .F. ) ;
#1982 = DIRECTION ( 'NONE',  ( 0.000000000000000000, 0.000000000000000000, 1.000000000000000000 ) ) ;
#1983 = ORIENTED_EDGE ( 'NONE', *, *, #340, .F. ) ;
#1984 = CARTESIAN_POINT ( 'NONE',  ( -1.878215178125000939, -25.96562499938548285, 12.25316411605952283 ) ) ;
#1985 = EDGE_LOOP ( 'NONE', ( #611, #6697, #5907, #16169 ) ) ;
#1986 = CARTESIAN_POINT ( 'NONE',  ( 1.071796769724494336, 25.48615380933863150, 4.999999999999992895 ) ) ;
#1987 = ORIENTED_EDGE ( 'NONE', *, *, #23515, .F. ) ;
#1988 = FACE_OUTER_BOUND ( 'NONE', #18323, .T. ) ;
#1989 = CARTESIAN_POINT ( 'NONE',  ( 3.735045420075836212E-15, 27.16562499938547859, 4.662447845253954171 ) ) ;
#1990 = CARTESIAN_POINT ( 'NONE',  ( 1.878215178125000939, -12.25316411605952283, 1.078124999385483784 ) ) ;
#1991 = DIRECTION ( 'NONE',  ( 0.000000000000000000, 0.000000000000000000, -1.000000000000000000 ) ) ;
#1992 = CARTESIAN_POINT ( 'NONE',  ( 19.44764619088677549, 19.44764619088670088, 4.662447845253954171 ) ) ;
#1993 = DIRECTION ( 'NONE',  ( 1.000000000000000000, 0.000000000000000000, 0.000000000000000000 ) ) ;
#1994 = CARTESIAN_POINT ( 'NONE',  ( 3.834746474454188013E-15, 26.01249999999999574, 4.999999999999992006 ) ) ;
#1995 = AXIS2_PLACEMENT_3D ( 'NONE', #7561, #7812, #17496 ) ;
#1996 = CARTESIAN_POINT ( 'NONE',  ( -3.999999999999996003, 26.98750000000000426, 6.690598923241487306 ) ) ;
#1997 = CARTESIAN_POINT ( 'NONE',  ( 24.86329371854774806, 18.68225429291723216, -6.500000000000000000 ) ) ;
#1998 = DIRECTION ( 'NONE',  ( -0.000000000000000000, -0.000000000000000000, 1.000000000000000000 ) ) ;
#1999 =( BOUNDED_CURVE ( )  B_SPLINE_CURVE ( 2, ( #3978, #22404, #8038, #17843, #21895, #20180, #13927, #19797, #1895 ),
 .UNSPECIFIED., .F., .F. ) 
 B_SPLINE_CURVE_WITH_KNOTS ( ( 3, 2, 2, 2, 3 ),
 ( 0.1250000000000000000, 0.1333333333333333315, 0.1499999999999999944, 0.1666666666666666574, 0.1749999999999999889 ),
 .UNSPECIFIED. ) 
 CURVE ( )  GEOMETRIC_REPRESENTATION_ITEM ( )  RATIONAL_B_SPLINE_CURVE ( ( 0.9330127018922194093, 0.9330127018922194093, 1.000000000000000000, 0.8660254037844387076, 1.000000000000000000, 0.8660254037844387076, 1.000000000000000000, 0.9330127018922194093, 0.9330127018922194093 ) ) 
 REPRESENTATION_ITEM ( '' )  );
#2000 = ORIENTED_EDGE ( 'NONE', *, *, #11892, .F. ) ;
#2001 = EDGE_CURVE ( 'NONE', #23534, #2876, #6355, .T. ) ;
#2002 = VERTEX_POINT ( 'NONE', #10132 ) ;
#2003 = CARTESIAN_POINT ( 'NONE',  ( -3.756430356249994773, 26.37812499938548783, 8.999999999999992895 ) ) ;
#2004 = ADVANCED_FACE ( 'NONE', ( #12092 ), #24395, .F. ) ;
#2005 = ORIENTED_EDGE ( 'NONE', *, *, #107, .F. ) ;
#2006 = DIRECTION ( 'NONE',  ( 0.000000000000000000, 0.000000000000000000, 1.000000000000000000 ) ) ;
#2007 = CARTESIAN_POINT ( 'NONE',  ( -3.999999999999996447, 29.66874999877096997, 8.999999999999992895 ) ) ;
#2008 = CARTESIAN_POINT ( 'NONE',  ( 2.672651547586948120E-15, 29.19062499938548783, 13.33755215474602984 ) ) ;
#2009 = CARTESIAN_POINT ( 'NONE',  ( 3.469446951953614189E-15, 31.50000000000000000, 8.999999999999992895 ) ) ;
#2010 = ORIENTED_EDGE ( 'NONE', *, *, #20661, .T. ) ;
#2011 = ADVANCED_FACE ( 'NONE', ( #20068 ), #2296, .F. ) ;
#2012 = EDGE_CURVE ( 'NONE', #11918, #25564, #21586, .T. ) ;
#2013 = CIRCLE ( 'NONE', #11178, 8.000000000000000000 ) ;
#2014 = DIRECTION ( 'NONE',  ( -0.9297764858882481276, 0.3681245526846864125, 0.000000000000000000 ) ) ;
#2015 = ORIENTED_EDGE ( 'NONE', *, *, #20840, .T. ) ;
#2016 = CARTESIAN_POINT ( 'NONE',  ( 0.4451413195716044102, 38.71736240459208034, 14.76550166049843149 ) ) ;
#2017 = CARTESIAN_POINT ( 'NONE',  ( 3.756430356250003655, 26.04062499938548569, 8.999999999999992895 ) ) ;
#2018 = DIRECTION ( 'NONE',  ( -0.000000000000000000, -1.000000000000000000, 0.000000000000000000 ) ) ;
#2019 = CIRCLE ( 'NONE', #6193, 31.10000000000000142 ) ;
#2020 = DIRECTION ( 'NONE',  ( 1.000000000000000000, 0.000000000000000000, 0.000000000000000000 ) ) ;
#2021 = FACE_OUTER_BOUND ( 'NONE', #9736, .T. ) ;
#2022 = CARTESIAN_POINT ( 'NONE',  ( 4.000000000000000888, 26.31250000000000711, 11.30940107675849760 ) ) ;
#2023 = CARTESIAN_POINT ( 'NONE',  ( -3.756430356249997882, 26.75312499938548427, 11.16877607737301226 ) ) ;
#2024 = CARTESIAN_POINT ( 'NONE',  ( 8.831537335106614961E-15, 27.13750000000000284, 12.99999999999999112 ) ) ;
#2025 = DIRECTION ( 'NONE',  ( 0.000000000000000000, 0.000000000000000000, -1.000000000000000000 ) ) ;
#2026 = AXIS2_PLACEMENT_3D ( 'NONE', #14786, #18694, #781 ) ;
#2027 = AXIS2_PLACEMENT_3D ( 'NONE', #6618, #6887, #2580 ) ;
#2028 = LINE ( 'NONE', #15763, #18740 ) ;
#2029 = CARTESIAN_POINT ( 'NONE',  ( 19.82550637751786482, 19.82550637751779377, 13.61880215351699874 ) ) ;
#2030 = CARTESIAN_POINT ( 'NONE',  ( 3.756430356250004987, 29.64062499938548711, 8.999999999999992895 ) ) ;
#2031 = DIRECTION ( 'NONE',  ( -0.000000000000000000, 0.000000000000000000, -1.000000000000000000 ) ) ;
#2032 = CARTESIAN_POINT ( 'NONE',  ( 1.999999999999995781, -27.79374999877096997, 5.535898384862237620 ) ) ;
#2035 = EDGE_CURVE ( 'NONE', #14487, #10748, #9232, .T. ) ;
#2034 = CARTESIAN_POINT ( 'NONE',  ( 3.756430356249997438, -25.85312499938548569, 11.16877607737301048 ) ) ;
#2033 = CIRCLE ( 'NONE', #10360, 0.5000000000000003331 ) ;
#2036 = CARTESIAN_POINT ( 'NONE',  ( 20.56133937125558830, 20.56133937125551370, 13.33755215474603162 ) ) ;
#2037 = CIRCLE ( 'NONE', #10361, 0.5000000000000000000 ) ;
#2038 = ORIENTED_EDGE ( 'NONE', *, *, #14019, .F. ) ;
#2039 = CARTESIAN_POINT ( 'NONE',  ( 2.000000000000000888, 27.56874999877096855, 12.46410161513774817 ) ) ;
#2040 = CARTESIAN_POINT ( 'NONE',  ( -4.000000000000003553, -27.73750000000000071, 6.690598923241489970 ) ) ;
#2042 = VERTEX_POINT ( 'NONE', #10371 ) ;
#2041 = CARTESIAN_POINT ( 'NONE',  ( -3.756430356249996549, 27.27812499938548996, 8.999999999999992895 ) ) ;
#2043 = CARTESIAN_POINT ( 'NONE',  ( 3.756430356250003211, 27.99062499938548498, 6.831223922626973533 ) ) ;
#2044 = LINE ( 'NONE', #1799, #1322 ) ;
#2045 = CARTESIAN_POINT ( 'NONE',  ( 31.03863125411924173, -1.952785157361756951, 1.000000000000000000 ) ) ;
#2046 = DIRECTION ( 'NONE',  ( -0.000000000000000000, -0.000000000000000000, -1.000000000000000000 ) ) ;
#2047 = EDGE_LOOP ( 'NONE', ( #7063, #21624, #23983, #13118 ) ) ;
#2048 = VERTEX_POINT ( 'NONE', #16429 ) ;
#2049 = DIRECTION ( 'NONE',  ( -0.7289686274214168815, -0.6845471059286831750, 0.000000000000000000 ) ) ;
#2050 = CARTESIAN_POINT ( 'NONE',  ( 1.878215178125005158, 28.81562499938548783, 5.746835883940462963 ) ) ;
#2051 =( BOUNDED_CURVE ( )  B_SPLINE_CURVE ( 2, ( #6648, #14634, #22615, #4703, #10569, #651, #16728 ),
 .UNSPECIFIED., .F., .F. ) 
 B_SPLINE_CURVE_WITH_KNOTS ( ( 3, 2, 2, 3 ),
 ( 0.6500000000000002442, 0.6666666666666668517, 0.6833333333333335702, 0.7000000000000001776 ),
 .UNSPECIFIED. ) 
 CURVE ( )  GEOMETRIC_REPRESENTATION_ITEM ( )  RATIONAL_B_SPLINE_CURVE ( ( 0.9999999999999982236, 0.8660254037844404840, 1.000000000000000000, 0.8660254037844387076, 1.000000000000000000, 0.8660254037844369313, 1.000000000000001776 ) ) 
 REPRESENTATION_ITEM ( '' )  );
#2052 = EDGE_CURVE ( 'NONE', #22340, #17898, #23384, .T. ) ;
#2053 = VECTOR ( 'NONE', #21376, 1000.000000000000000 ) ;
#2054 = AXIS2_PLACEMENT_3D ( 'NONE', #23317, #25026, #25407 ) ;
#2055 = CARTESIAN_POINT ( 'NONE',  ( 3.756430356250002323, -11.16877607737301403, 4.153124999385482852 ) ) ;
#2056 = AXIS2_PLACEMENT_3D ( 'NONE', #10382, #612, #6602 ) ;
#2057 = AXIS2_PLACEMENT_3D ( 'NONE', #24683, #18412, #24817 ) ;
#2058 = CARTESIAN_POINT ( 'NONE',  ( -0.7500000000000001110, 20.00000000000000000, 17.69999999999999929 ) ) ;
#2059 = CARTESIAN_POINT ( 'NONE',  ( 2.620986760973688460E-15, -13.61880215351699874, 3.937499999999998224 ) ) ;
#2060 = DIRECTION ( 'NONE',  ( 0.000000000000000000, 0.000000000000000000, 1.000000000000000000 ) ) ;
#2061 = DIRECTION ( 'NONE',  ( -0.000000000000000000, -1.000000000000000000, -0.000000000000000000 ) ) ;
#2062 = CARTESIAN_POINT ( 'NONE',  ( 1.071796769724494558, 25.54240381056766651, 4.999999999999992895 ) ) ;
#2063 = CARTESIAN_POINT ( 'NONE',  ( -3.110308778861273105, 38.49999999999999289, 14.13088484572967118 ) ) ;
#2064 = CARTESIAN_POINT ( 'NONE',  ( 17.48763458135079318, 23.14448883084309472, 6.690598923241487306 ) ) ;
#2065 = ORIENTED_EDGE ( 'NONE', *, *, #10383, .F. ) ;
#2066 = CARTESIAN_POINT ( 'NONE',  ( -5.201336420084783363, 38.97860908142765624, 10.85357947325328176 ) ) ;
#2067 = DIRECTION ( 'NONE',  ( 0.000000000000000000, -0.000000000000000000, 1.000000000000000000 ) ) ;
#2068 = CARTESIAN_POINT ( 'NONE',  ( -3.756430356249996994, 28.17812499938548498, 8.999999999999992895 ) ) ;
#2069 = AXIS2_PLACEMENT_3D ( 'NONE', #25572, #23104, #3093 ) ;
#2070 = CARTESIAN_POINT ( 'NONE',  ( -1.999999999999995781, -5.535898384862237620, 2.399999999999999467 ) ) ;
#2071 = CARTESIAN_POINT ( 'NONE',  ( 3.834746474454188013E-15, 26.40624999877096357, 4.999999999999992006 ) ) ;
#2072 = CARTESIAN_POINT ( 'NONE',  ( 2.000000000000000888, 28.91874999877096997, 12.46410161513774817 ) ) ;
#2073 = ORIENTED_EDGE ( 'NONE', *, *, #8131, .F. ) ;
#2074 = CARTESIAN_POINT ( 'NONE',  ( 1.071796769724491227, 27.28615380933863577, 4.999999999999989342 ) ) ;
#2075 = CARTESIAN_POINT ( 'NONE',  ( -3.999999999999997335, 26.10624999877096997, 11.30940107675849404 ) ) ;
#2076 = DIRECTION ( 'NONE',  ( 0.000000000000000000, -1.000000000000000000, 0.000000000000000000 ) ) ;
#2078 = VERTEX_POINT ( 'NONE', #2171 ) ;
#2077 = CARTESIAN_POINT ( 'NONE',  ( 0.000000000000000000, 0.000000000000000000, -6.500000000000000000 ) ) ;
#2080 = ORIENTED_EDGE ( 'NONE', *, *, #18735, .T. ) ;
#2079 = AXIS2_PLACEMENT_3D ( 'NONE', #5171, #16819, #2941 ) ;
#2082 = EDGE_CURVE ( 'NONE', #15046, #10411, #11305, .T. ) ;
#2081 = ORIENTED_EDGE ( 'NONE', *, *, #7267, .T. ) ;
#2083 = VERTEX_POINT ( 'NONE', #16289 ) ;
#2084 = CARTESIAN_POINT ( 'NONE',  ( 0.000000000000000000, 20.00000000000000000, 18.19999999999999929 ) ) ;
#2085 = CARTESIAN_POINT ( 'NONE',  ( -20.92219106202026069, 23.01025686871660980, 1.000000000000000000 ) ) ;
#2086 = CIRCLE ( 'NONE', #4169, 0.5000000000000005551 ) ;
#2087 = DIRECTION ( 'NONE',  ( 1.000000000000000000, 0.000000000000000000, 0.000000000000000000 ) ) ;
#2089 = EDGE_CURVE ( 'NONE', #25409, #23573, #13729, .T. ) ;
#2088 = CARTESIAN_POINT ( 'NONE',  ( -3.756430356249996549, 27.61562499938548143, 8.999999999999992895 ) ) ;
#2090 = CIRCLE ( 'NONE', #3756, 0.4999999999999998890 ) ;
#2091 = CARTESIAN_POINT ( 'NONE',  ( 1.878215178125000939, -12.25316411605952283, 4.115624999385482319 ) ) ;
#2092 = CARTESIAN_POINT ( 'NONE',  ( -1.999999999999998224, -12.46410161513774639, 4.293749998770968190 ) ) ;
#2093 =( NAMED_UNIT ( * ) SI_UNIT ( $, .STERADIAN. ) SOLID_ANGLE_UNIT ( ) );
#2094 = CARTESIAN_POINT ( 'NONE',  ( -3.756430356249996994, 25.36562499938548498, 8.999999999999992895 ) ) ;
#2095 = CARTESIAN_POINT ( 'NONE',  ( 18.27871029367229383, 21.10713741841841085, 5.535898384862237620 ) ) ;
#2096 = DIRECTION ( 'NONE',  ( 1.000000000000000000, 0.000000000000000000, 0.000000000000000000 ) ) ;
#2097 = CARTESIAN_POINT ( 'NONE',  ( 3.756430356250003211, 25.17812499938548498, 6.831223922626973533 ) ) ;
#2098 = CYLINDRICAL_SURFACE ( 'NONE', #17997, 0.5000000000000004441 ) ;
#2099 = DIRECTION ( 'NONE',  ( 0.000000000000000000, 0.000000000000000000, 1.000000000000000000 ) ) ;
#2100 = CARTESIAN_POINT ( 'NONE',  ( 0.000000000000000000, 0.000000000000000000, 1.000000000000000000 ) ) ;
#2101 = CARTESIAN_POINT ( 'NONE',  ( -3.752267015613588906E-15, -28.65624999877096712, 4.381197846482986158 ) ) ;
#2102 = CARTESIAN_POINT ( 'NONE',  ( 3.756430356250004099, 27.54062499938548569, 6.831223922626973533 ) ) ;
#2103 = DIRECTION ( 'NONE',  ( -0.06279051952930156388, 0.9980267284282724471, 0.000000000000000000 ) ) ;
#2104 = VECTOR ( 'NONE', #14071, 1000.000000000000000 ) ;
#2105 = CARTESIAN_POINT ( 'NONE',  ( -1.999999999999998224, 29.74374999877096926, 12.46410161513774639 ) ) ;
#2106 = DIRECTION ( 'NONE',  ( -0.000000000000000000, 0.000000000000000000, 1.000000000000000000 ) ) ;
#2107 = EDGE_LOOP ( 'NONE', ( #7495, #22644, #3467, #8386 ) ) ;
#2109 = ORIENTED_EDGE ( 'NONE', *, *, #21512, .F. ) ;
#2108 = CARTESIAN_POINT ( 'NONE',  ( -1.878215178125004048, -28.81562499938548427, 5.746835883940462963 ) ) ;
#2110 = COLOUR_RGB ( '',0.8941176470588234615, 0.8941176470588234615, 0.8941176470588234615 ) ;
#2111 = AXIS2_PLACEMENT_3D ( 'NONE', #16330, #4155, #8480 ) ;
#2113 = EDGE_LOOP ( 'NONE', ( #13094, #10552, #24464, #2081 ) ) ;
#2112 = ADVANCED_FACE ( 'NONE', ( #10641 ), #21477, .T. ) ;
#2114 = CYLINDRICAL_SURFACE ( 'NONE', #6645, 4.000000000000000000 ) ;
#2115 = ORIENTED_EDGE ( 'NONE', *, *, #25617, .F. ) ;
#2116 = VERTEX_POINT ( 'NONE', #5258 ) ;
#2117 = ORIENTED_EDGE ( 'NONE', *, *, #6935, .T. ) ;
#2118 = CARTESIAN_POINT ( 'NONE',  ( 2.000000000000003997, -5.535898384862238508, 2.718749998770968013 ) ) ;
#2119 = AXIS2_PLACEMENT_3D ( 'NONE', #7456, #13612, #1457 ) ;
#2120 = EDGE_CURVE ( 'NONE', #8878, #5837, #20859, .T. ) ;
#2121 = EDGE_LOOP ( 'NONE', ( #9027, #1692, #19353, #14919 ) ) ;
#2122 = EDGE_CURVE ( 'NONE', #23121, #13852, #15327, .T. ) ;
#2123 = CARTESIAN_POINT ( 'NONE',  ( -25.16042852506104666, -18.28012134629567598, -6.500000000000000000 ) ) ;
#2124 = CARTESIAN_POINT ( 'NONE',  ( 3.756430356250002323, 26.11562499938548498, 11.16877607737301403 ) ) ;
#2125 = DIRECTION ( 'NONE',  ( -0.3681245526846803617, -0.9297764858882504591, 0.000000000000000000 ) ) ;
#2126 = DIRECTION ( 'NONE',  ( -0.000000000000000000, -1.000000000000000000, -0.000000000000000000 ) ) ;
#2127 = CARTESIAN_POINT ( 'NONE',  ( 16.55280027427694378, 21.86519503019561839, 8.999999999999992895 ) ) ;
#2128 = EDGE_CURVE ( 'NONE', #23884, #11133, #10823, .T. ) ;
#2129 = VECTOR ( 'NONE', #20230, 1000.000000000000000 ) ;
#2130 = CARTESIAN_POINT ( 'NONE',  ( 4.000000000000003553, -8.999999999999992895, 0.000000000000000000 ) ) ;
#2131 = CIRCLE ( 'NONE', #16756, 31.10000000000000142 ) ;
#2132 = DIRECTION ( 'NONE',  ( -0.000000000000000000, -0.000000000000000000, -1.000000000000000000 ) ) ;
#2133 = CONTEXT_DEPENDENT_SHAPE_REPRESENTATION ( #21619, #24907 ) ;
#2134 = CARTESIAN_POINT ( 'NONE',  ( -1.878215178124998497, -12.25316411605951927, 1.790624999385481697 ) ) ;
#2135 = CARTESIAN_POINT ( 'NONE',  ( -3.999999999999997335, 28.41249999999999787, 11.30940107675849404 ) ) ;
#2136 = AXIS2_PLACEMENT_3D ( 'NONE', #11970, #15915, #24406 ) ;
#2137 = CARTESIAN_POINT ( 'NONE',  ( 3.756430356250003655, 28.29062499938548569, 8.999999999999992895 ) ) ;
#2138 = CYLINDRICAL_SURFACE ( 'NONE', #3780, 4.000000000000000000 ) ;
#2139 = CARTESIAN_POINT ( 'NONE',  ( 17.87862548900172399, 23.19102024492039504, 6.831223922626973533 ) ) ;
#2140 = CARTESIAN_POINT ( 'NONE',  ( 0.7500000000000000000, -1.299038105676658450, 17.69999999999999929 ) ) ;
#2141 = ORIENTED_EDGE ( 'NONE', *, *, #7653, .F. ) ;
#2142 = ORIENTED_EDGE ( 'NONE', *, *, #19912, .T. ) ;
#2143 = CARTESIAN_POINT ( 'NONE',  ( 4.006172263299091013E-15, 26.71562499938548996, 4.662447845253954171 ) ) ;
#2144 = CIRCLE ( 'NONE', #20503, 0.5000000000000007772 ) ;
#2145 = VERTEX_POINT ( 'NONE', #9561 ) ;
#2146 = DIRECTION ( 'NONE',  ( 1.000000000000000000, 0.000000000000000000, 0.000000000000000000 ) ) ;
#2147 = CARTESIAN_POINT ( 'NONE',  ( 2.620986760973688460E-15, 29.33124999877096784, 13.61880215351699874 ) ) ;
#2148 = CARTESIAN_POINT ( 'NONE',  ( 4.000000000000003553, -8.999999999999992895, 0.3937499987709675020 ) ) ;
#2149 = CARTESIAN_POINT ( 'NONE',  ( 3.834746474454188013E-15, 26.01249999999999574, 4.999999999999992006 ) ) ;
#2150 = ORIENTED_EDGE ( 'NONE', *, *, #3374, .T. ) ;
#2151 = CIRCLE ( 'NONE', #16363, 30.10000000000000142 ) ;
#2152 = CARTESIAN_POINT ( 'NONE',  ( -3.469446951953614189E-15, -30.00000000000000355, 8.999999999999992895 ) ) ;
#2153 = VERTEX_POINT ( 'NONE', #16671 ) ;
#2154 = DIRECTION ( 'NONE',  ( 0.000000000000000000, -0.000000000000000000, 1.000000000000000000 ) ) ;
#2155 = CARTESIAN_POINT ( 'NONE',  ( 1.878215178125004048, 26.56562499938548427, 5.746835883940462963 ) ) ;
#2156 = DIRECTION ( 'NONE',  ( 0.9297764858882561212, 0.3681245526846659843, 0.000000000000000000 ) ) ;
#2157 = AXIS2_PLACEMENT_3D ( 'NONE', #21135, #23345, #11317 ) ;
#2158 = DIRECTION ( 'NONE',  ( -0.7071067811865487940, -0.7071067811865463515, 0.000000000000000000 ) ) ;
#2159 = CARTESIAN_POINT ( 'NONE',  ( 2.000000000000000000, 28.52500000000000924, 12.46410161513774817 ) ) ;
#2160 = EDGE_CURVE ( 'NONE', #3679, #5799, #13370, .T. ) ;
#2161 = EDGE_CURVE ( 'NONE', #17006, #8351, #10005, .T. ) ;
#2162 = VECTOR ( 'NONE', #14829, 1000.000000000000000 ) ;
#2163 = CARTESIAN_POINT ( 'NONE',  ( -3.756430356249997882, 26.30312499938548498, 11.16877607737301226 ) ) ;
#2164 = CIRCLE ( 'NONE', #24280, 8.000000000000000000 ) ;
#2165 = CIRCLE ( 'NONE', #18881, 31.10000000000000142 ) ;
#2166 = CARTESIAN_POINT ( 'NONE',  ( 25.16042852506077665, -18.28012134629603835, -6.500000000000000000 ) ) ;
#2167 = DIRECTION ( 'NONE',  ( 0.000000000000000000, 0.000000000000000000, 1.000000000000000000 ) ) ;
#2168 = CARTESIAN_POINT ( 'NONE',  ( 23.05168106668148553, 17.39482681718902768, 8.999999999999992895 ) ) ;
#2169 = DIRECTION ( 'NONE',  ( -0.000000000000000000, -0.000000000000000000, 1.000000000000000000 ) ) ;
#2170 = CARTESIAN_POINT ( 'NONE',  ( -15.41874213889376044, 27.00874656207322388, 1.000000000000000000 ) ) ;
#2171 = CARTESIAN_POINT ( 'NONE',  ( -30.63887302793251521, -5.335677986744475021, -6.500000000000000000 ) ) ;
#2172 = VECTOR ( 'NONE', #16285, 1000.000000000000000 ) ;
#2173 = DIRECTION ( 'NONE',  ( -0.000000000000000000, -0.000000000000000000, 1.000000000000000000 ) ) ;
#2174 = LINE ( 'NONE', #10135, #11663 ) ;
#2175 = VERTEX_POINT ( 'NONE', #24639 ) ;
#2176 = CARTESIAN_POINT ( 'NONE',  ( -3.999999999999996447, 28.31874999877096855, 8.999999999999992895 ) ) ;
#2177 = CARTESIAN_POINT ( 'NONE',  ( -2.000000000000003997, -28.67500000000000426, 5.535898384862238508 ) ) ;
#2179 = ORIENTED_EDGE ( 'NONE', *, *, #17336, .F. ) ;
#2178 = CARTESIAN_POINT ( 'NONE',  ( -3.756430356249996549, 26.34062499938548285, 6.831223922626973533 ) ) ;
#2180 = CARTESIAN_POINT ( 'NONE',  ( 1.878215178125000939, 28.32812499938548711, 12.25316411605952283 ) ) ;
#2181 = DIRECTION ( 'NONE',  ( -0.000000000000000000, -0.000000000000000000, 1.000000000000000000 ) ) ;
#2182 = DIRECTION ( 'NONE',  ( 0.000000000000000000, 0.000000000000000000, 1.000000000000000000 ) ) ;
#2183 = ORIENTED_EDGE ( 'NONE', *, *, #9367, .F. ) ;
#2184 = ORIENTED_EDGE ( 'NONE', *, *, #24522, .F. ) ;
#2185 = DIRECTION ( 'NONE',  ( 0.000000000000000000, 0.000000000000000000, 1.000000000000000000 ) ) ;
#2186 = VECTOR ( 'NONE', #23671, 1000.000000000000000 ) ;
#2187 = CARTESIAN_POINT ( 'NONE',  ( 3.756430356250002323, 27.80312499938548854, 11.16877607737301226 ) ) ;
#2188 = CARTESIAN_POINT ( 'NONE',  ( 20.69613160098474580, 17.86770447623847957, 5.535898384862238508 ) ) ;
#2189 = AXIS2_PLACEMENT_3D ( 'NONE', #23804, #15712, #12018 ) ;
#2190 = ADVANCED_FACE ( 'NONE', ( #18636 ), #22697, .F. ) ;
#2191 = CARTESIAN_POINT ( 'NONE',  ( -1.878215178124995832, -5.746835883940462963, 2.090624999385483296 ) ) ;
#2192 = VECTOR ( 'NONE', #21248, 1000.000000000000000 ) ;
#2193 = CIRCLE ( 'NONE', #16817, 5.500000000000000000 ) ;
#2194 = ADVANCED_FACE ( 'NONE', ( #2802 ), #19494, .T. ) ;
#2195 = CARTESIAN_POINT ( 'NONE',  ( -1.999999999999994893, 28.24374999877096926, 5.535898384862237620 ) ) ;
#2196 = CARTESIAN_POINT ( 'NONE',  ( 3.999999999999956035, -11.30940107675852602, 4.012499999999995737 ) ) ;
#2197 = DIRECTION ( 'NONE',  ( 0.000000000000000000, 0.000000000000000000, -1.000000000000000000 ) ) ;
#2198 = AXIS2_PLACEMENT_3D ( 'NONE', #18811, #10567, #899 ) ;
#2199 = CARTESIAN_POINT ( 'NONE',  ( -19.32388608118395013, 23.96296185032730364, -6.500000000000000000 ) ) ;
#2200 = CARTESIAN_POINT ( 'NONE',  ( 19.46311415215975771, 16.63468702741349858, 5.535898384862238508 ) ) ;
#2201 = CARTESIAN_POINT ( 'NONE',  ( -5.335677986744340906, 30.63887302793254364, -2.750000000000000000 ) ) ;
#2202 = CARTESIAN_POINT ( 'NONE',  ( 17.85665593321704137, 17.85665593321697742, 4.662447845253954171 ) ) ;
#2203 = CARTESIAN_POINT ( 'NONE',  ( 19.46753356867311524, 19.46753356867304774, 13.61880215351699874 ) ) ;
#2204 = EDGE_CURVE ( 'NONE', #2274, #9390, #19188, .T. ) ;
#2205 = ORIENTED_EDGE ( 'NONE', *, *, #4303, .F. ) ;
#2206 = CARTESIAN_POINT ( 'NONE',  ( 3.469446951953614189E-15, 39.50000000000000000, 8.999999999999992895 ) ) ;
#2207 = CARTESIAN_POINT ( 'NONE',  ( 5.442264176411883980, 38.59882996731582239, 6.718392883288001549 ) ) ;
#2208 = CARTESIAN_POINT ( 'NONE',  ( -3.756430356249996994, 25.36562499938548498, 8.999999999999992895 ) ) ;
#2209 = AXIS2_PLACEMENT_3D ( 'NONE', #23562, #4189, #23679 ) ;
#2210 = CARTESIAN_POINT ( 'NONE',  ( 3.469446951953614189E-15, 30.00000000000000355, 4.999999999999992006 ) ) ;
#2211 = CARTESIAN_POINT ( 'NONE',  ( -2.451530025009224456, -31.00322564728513086, 1.000000000000000000 ) ) ;
#2212 = CARTESIAN_POINT ( 'NONE',  ( 23.83066714524420249, 18.34604264253855987, 8.999999999999992895 ) ) ;
#2213 = ORIENTED_EDGE ( 'NONE', *, *, #1809, .F. ) ;
#2214 = CARTESIAN_POINT ( 'NONE',  ( 0.000000000000000000, 0.000000000000000000, -6.500000000000000000 ) ) ;
#2215 = CARTESIAN_POINT ( 'NONE',  ( 3.752267015613588906E-15, 26.40624999877097068, 4.381197846482986158 ) ) ;
#2216 = CARTESIAN_POINT ( 'NONE',  ( -2.672651547586948120E-15, -26.37812499938548427, 13.33755215474602984 ) ) ;
#2218 = ORIENTED_EDGE ( 'NONE', *, *, #14683, .F. ) ;
#2217 = DIRECTION ( 'NONE',  ( -1.000000000000000000, 0.000000000000000000, 0.000000000000000000 ) ) ;
#2219 = EDGE_LOOP ( 'NONE', ( #9954, #6871, #760, #24291 ) ) ;
#2220 = VERTEX_POINT ( 'NONE', #21343 ) ;
#2221 = EDGE_LOOP ( 'NONE', ( #25871, #19213, #10345, #5237 ) ) ;
#2222 = DIRECTION ( 'NONE',  ( 1.000000000000000000, 0.000000000000000000, 0.000000000000000000 ) ) ;
#2223 = AXIS2_PLACEMENT_3D ( 'NONE', #18502, #16537, #24500 ) ;
#2224 =( LENGTH_UNIT ( ) NAMED_UNIT ( * ) SI_UNIT ( .MILLI., .METRE. ) );
#2225 = EDGE_CURVE ( 'NONE', #11292, #18617, #20028, .T. ) ;
#2226 = CARTESIAN_POINT ( 'NONE',  ( -1.878215178124996498, 26.19062499938548783, 5.746835883940462963 ) ) ;
#2227 = CARTESIAN_POINT ( 'NONE',  ( -1.878215178124995832, -5.746835883940462963, 4.340624999385481964 ) ) ;
#2228 = CARTESIAN_POINT ( 'NONE',  ( -1.999999999999995781, -5.535898384862237620, 3.693749998770968546 ) ) ;
#2229 = CARTESIAN_POINT ( 'NONE',  ( -3.756430356249995661, 25.32812499938548356, 6.831223922626973533 ) ) ;
#2230 = EDGE_CURVE ( 'NONE', #19514, #17747, #25386, .T. ) ;
#2231 = LINE ( 'NONE', #16354, #4218 ) ;
#2232 = DIRECTION ( 'NONE',  ( 0.000000000000000000, 0.000000000000000000, 1.000000000000000000 ) ) ;
#2233 = AXIS2_PLACEMENT_3D ( 'NONE', #13758, #15729, #7485 ) ;
#2234 = CARTESIAN_POINT ( 'NONE',  ( -3.756430356249996105, 25.32812499938548356, 6.831223922626973533 ) ) ;
#2235 = CARTESIAN_POINT ( 'NONE',  ( -30.12293631110050995, -7.734255490826679846, -6.500000000000000000 ) ) ;
#2236 = CARTESIAN_POINT ( 'NONE',  ( 2.000000000000000000, 26.21874999877097423, 12.46410161513774817 ) ) ;
#2237 = CARTESIAN_POINT ( 'NONE',  ( 18.07541709408115693, 18.07541709408108588, 4.999999999999992006 ) ) ;
#2238 = CARTESIAN_POINT ( 'NONE',  ( 1.999999999999995781, -29.14374999877096784, 5.535898384862237620 ) ) ;
#2239 = CARTESIAN_POINT ( 'NONE',  ( 3.834746474454188013E-15, 27.36250000000000071, 4.999999999999992006 ) ) ;
#2241 = EDGE_CURVE ( 'NONE', #5871, #345, #15594, .T. ) ;
#2240 = CARTESIAN_POINT ( 'NONE',  ( 0.000000000000000000, 0.000000000000000000, -6.500000000000000000 ) ) ;
#2242 = DIRECTION ( 'NONE',  ( 0.000000000000000000, 0.000000000000000000, 1.000000000000000000 ) ) ;
#2243 = CARTESIAN_POINT ( 'NONE',  ( 3.595210675795415867, -29.78396494222454294, 7.227341970420264161 ) ) ;
#2244 = VERTEX_POINT ( 'NONE', #15462 ) ;
#2245 = CARTESIAN_POINT ( 'NONE',  ( -3.401318489841309578, -30.91344420362545264, -2.750000000000000000 ) ) ;
#2247 = ORIENTED_EDGE ( 'NONE', *, *, #7336, .F. ) ;
#2246 = LINE ( 'NONE', #10201, #8730 ) ;
#2248 = ORIENTED_EDGE ( 'NONE', *, *, #24328, .T. ) ;
#2249 = ORIENTED_EDGE ( 'NONE', *, *, #1789, .F. ) ;
#2250 = ORIENTED_EDGE ( 'NONE', *, *, #3988, .T. ) ;
#2251 = VERTEX_POINT ( 'NONE', #21208 ) ;
#2252 = CARTESIAN_POINT ( 'NONE',  ( 19.98460540328483859, 19.98460540328476398, 4.999999999999992006 ) ) ;
#2253 = PRESENTATION_LAYER_ASSIGNMENT (  '', '', ( #1825 ) ) ;
#2254 = VERTEX_POINT ( 'NONE', #17304 ) ;
#2255 = CARTESIAN_POINT ( 'NONE',  ( 2.620986760973688460E-15, 28.93750000000000000, 13.61880215351699874 ) ) ;
#2256 = CARTESIAN_POINT ( 'NONE',  ( 3.756430356250003655, 25.25312499938548427, 8.999999999999992895 ) ) ;
#2257 = CIRCLE ( 'NONE', #16886, 31.10000000000000142 ) ;
#2258 = CARTESIAN_POINT ( 'NONE',  ( 3.756430356250002323, -11.16877607737301226, 2.015624999385483118 ) ) ;
#2259 = FACE_OUTER_BOUND ( 'NONE', #17250, .T. ) ;
#2260 = CARTESIAN_POINT ( 'NONE',  ( 17.21571288163933389, 22.52810763755800849, 11.16877607737301226 ) ) ;
#2261 = DIRECTION ( 'NONE',  ( 0.3681245526846875782, 0.9297764858882475725, 0.000000000000000000 ) ) ;
#2262 = EDGE_CURVE ( 'NONE', #15216, #21568, #413, .T. ) ;
#2263 = FACE_OUTER_BOUND ( 'NONE', #14410, .T. ) ;
#2264 = CARTESIAN_POINT ( 'NONE',  ( 3.756430356250003655, -8.999999999999992895, 2.390624999385481342 ) ) ;
#2265 = CARTESIAN_POINT ( 'NONE',  ( -0.4999838450259763700, 31.09598070739550124, -2.750000000000000000 ) ) ;
#2266 = CARTESIAN_POINT ( 'NONE',  ( 1.878215178125000939, 28.66562499938548569, 12.25316411605952283 ) ) ;
#2267 = CARTESIAN_POINT ( 'NONE',  ( 3.469446951953614189E-15, -8.999999999999992895, 0.000000000000000000 ) ) ;
#2268 = EDGE_CURVE ( 'NONE', #7474, #12702, #12622, .T. ) ;
#2269 = CARTESIAN_POINT ( 'NONE',  ( 15.31328122920215229, 20.97013547869446626, 11.30940107675849404 ) ) ;
#2270 = FACE_OUTER_BOUND ( 'NONE', #11908, .T. ) ;
#2271 = VERTEX_POINT ( 'NONE', #18756 ) ;
#2272 = ORIENTED_EDGE ( 'NONE', *, *, #6192, .F. ) ;
#2273 = CARTESIAN_POINT ( 'NONE',  ( 3.756430356250004987, 27.95312499938548711, 8.999999999999992895 ) ) ;
#2274 = VERTEX_POINT ( 'NONE', #7473 ) ;
#2275 = CARTESIAN_POINT ( 'NONE',  ( -30.54913349766228592, -5.827558883615738594, 1.000000000000000000 ) ) ;
#2276 = ORIENTED_EDGE ( 'NONE', *, *, #7804, .F. ) ;
#2277 = CARTESIAN_POINT ( 'NONE',  ( -1.071796769724485454, 27.51115380933863719, 12.99999999999999467 ) ) ;
#2278 = EDGE_CURVE ( 'NONE', #11678, #7709, #7918, .T. ) ;
#2279 = ORIENTED_EDGE ( 'NONE', *, *, #13815, .F. ) ;
#2280 = LINE ( 'NONE', #19913, #10677 ) ;
#2281 = ORIENTED_EDGE ( 'NONE', *, *, #6066, .F. ) ;
#2282 = CARTESIAN_POINT ( 'NONE',  ( -0.3338636427494882097, 38.86740601410824780, 14.62281502694621871 ) ) ;
#2283 = CARTESIAN_POINT ( 'NONE',  ( -1.878215178124998497, 28.14062499938548356, 12.25316411605951927 ) ) ;
#2284 =( BOUNDED_CURVE ( )  B_SPLINE_CURVE ( 2, ( #17493, #3372, #7421, #11350, #7306, #9395, #23514, #13578, #7178 ),
 .UNSPECIFIED., .F., .T. ) 
 B_SPLINE_CURVE_WITH_KNOTS ( ( 3, 2, 2, 2, 3 ),
 ( 0.4250000000000000444, 0.4333333333333333481, 0.4500000000000000111, 0.4666666666666666741, 0.4750000000000000333 ),
 .UNSPECIFIED. ) 
 CURVE ( )  GEOMETRIC_REPRESENTATION_ITEM ( )  RATIONAL_B_SPLINE_CURVE ( ( 0.9330127018922194093, 0.9330127018922196314, 1.000000000000000000, 0.8660254037844387076, 1.000000000000000000, 0.8660254037844387076, 1.000000000000000000, 0.9330127018922191873, 0.9330127018922194093 ) ) 
 REPRESENTATION_ITEM ( '' )  );
#2285 = CARTESIAN_POINT ( 'NONE',  ( -1.057460391440397258E-14, 29.16249999999999787, 4.999999999999992006 ) ) ;
#2286 = CARTESIAN_POINT ( 'NONE',  ( 29.09636799667075024, -10.98232076577232519, -6.500000000000000000 ) ) ;
#2287 = CYLINDRICAL_SURFACE ( 'NONE', #22537, 31.10000000000000142 ) ;
#2288 = EDGE_CURVE ( 'NONE', #20963, #7544, #18242, .T. ) ;
#2289 = DIRECTION ( 'NONE',  ( 0.000000000000000000, 0.000000000000000000, 1.000000000000000000 ) ) ;
#2290 = CARTESIAN_POINT ( 'NONE',  ( 3.469446951953614189E-15, 35.50000000000000711, 8.999999999999992895 ) ) ;
#2291 = CARTESIAN_POINT ( 'NONE',  ( -26.50000000000000355, -0.5000000000000000000, 19.50000000000000000 ) ) ;
#2292 = CARTESIAN_POINT ( 'NONE',  ( 23.39639562250992810, 17.73954137301747380, 6.690598923241489970 ) ) ;
#2293 = DIRECTION ( 'NONE',  ( 0.000000000000000000, 0.000000000000000000, 1.000000000000000000 ) ) ;
#2294 = EDGE_CURVE ( 'NONE', #2754, #246, #2086, .T. ) ;
#2295 = CARTESIAN_POINT ( 'NONE',  ( 4.000000000000003553, -8.999999999999992895, 4.443749998770965881 ) ) ;
#2296 = CYLINDRICAL_SURFACE ( 'NONE', #5713, 4.000000000000000000 ) ;
#2297 = CARTESIAN_POINT ( 'NONE',  ( -1.878215178125004048, -25.21562499938548285, 5.746835883940462963 ) ) ;
#2298 = DIRECTION ( 'NONE',  ( 0.000000000000000000, 0.000000000000000000, -1.000000000000000000 ) ) ;
#2299 = ORIENTED_EDGE ( 'NONE', *, *, #18717, .T. ) ;
#2300 = CARTESIAN_POINT ( 'NONE',  ( 2.000000000000000888, 26.66874999877096641, 12.46410161513774817 ) ) ;
#2301 = CARTESIAN_POINT ( 'NONE',  ( -4.000000000000001776, -28.11250000000000426, 11.30940107675849760 ) ) ;
#2302 = EDGE_CURVE ( 'NONE', #2607, #25564, #21701, .T. ) ;
#2304 = VERTEX_POINT ( 'NONE', #6030 ) ;
#2303 = CARTESIAN_POINT ( 'NONE',  ( 3.756430356250006319, 27.99062499938548854, 6.831223922626973533 ) ) ;
#2305 = ORIENTED_EDGE ( 'NONE', *, *, #340, .T. ) ;
#2306 = LINE ( 'NONE', #10528, #24599 ) ;
#2307 = EDGE_CURVE ( 'NONE', #20603, #13396, #13885, .T. ) ;
#2308 = DIRECTION ( 'NONE',  ( 1.000000000000000000, 0.000000000000000000, 0.000000000000000000 ) ) ;
#2309 = CARTESIAN_POINT ( 'NONE',  ( 4.000000000000003553, 29.89374999877096784, 8.999999999999992895 ) ) ;
#2310 = ORIENTED_EDGE ( 'NONE', *, *, #17345, .T. ) ;
#2311 = ORIENTED_EDGE ( 'NONE', *, *, #12991, .F. ) ;
#2312 = CARTESIAN_POINT ( 'NONE',  ( -3.735045420075836212E-15, -26.71562499938548285, 4.662447845253954171 ) ) ;
#2313 = CARTESIAN_POINT ( 'NONE',  ( -3.756430356249998326, 27.20312499938549067, 11.16877607737301226 ) ) ;
#2314 = CARTESIAN_POINT ( 'NONE',  ( -31.09598070739550835, -0.4999838450256507416, -2.750000000000000000 ) ) ;
#2315 = CARTESIAN_POINT ( 'NONE',  ( 3.756430356250003211, -6.831223922626973533, 3.778124999385480631 ) ) ;
#2316 = CARTESIAN_POINT ( 'NONE',  ( 0.000000000000000000, 0.000000000000000000, 1.000000000000000000 ) ) ;
#2317 = DIRECTION ( 'NONE',  ( 0.000000000000000000, 0.000000000000000000, -1.000000000000000000 ) ) ;
#2318 = CARTESIAN_POINT ( 'NONE',  ( 20.26302869750798408, 20.26302869750790947, 4.999999999999992006 ) ) ;
#2319 = CARTESIAN_POINT ( 'NONE',  ( 25.98730014090442353, 17.08421000182768523, -2.750000000000000000 ) ) ;
#2320 = CARTESIAN_POINT ( 'NONE',  ( 1.071796769724495668, 26.65134618820330203, 12.99999999999999112 ) ) ;
#2321 = DIRECTION ( 'NONE',  ( 0.000000000000000000, -0.000000000000000000, 1.000000000000000000 ) ) ;
#2322 = CARTESIAN_POINT ( 'NONE',  ( 16.97933781724378122, 19.63553519520309010, 12.25316411605951927 ) ) ;
#2323 = CARTESIAN_POINT ( 'NONE',  ( 18.34500155353947903, 21.17342867828559605, 12.46410161513774639 ) ) ;
#2324 = ORIENTED_EDGE ( 'NONE', *, *, #620, .F. ) ;
#2325 = DIRECTION ( 'NONE',  ( 0.000000000000000000, -0.000000000000000000, 1.000000000000000000 ) ) ;
#2326 = DIRECTION ( 'NONE',  ( 1.000000000000000000, 0.000000000000000000, 0.000000000000000000 ) ) ;
#2327 = CARTESIAN_POINT ( 'NONE',  ( 3.756430356250002323, 29.26562499938548356, 11.16877607737301226 ) ) ;
#2329 = VERTEX_POINT ( 'NONE', #22103 ) ;
#2328 = CARTESIAN_POINT ( 'NONE',  ( -3.794751686895379894, 29.75919970560060079, 7.708599238039753665 ) ) ;
#2330 = CARTESIAN_POINT ( 'NONE',  ( 15.62472262396960154, 20.93711737988828148, 11.16877607737301048 ) ) ;
#2331 = CARTESIAN_POINT ( 'NONE',  ( 3.999999999999996447, -27.92500000000000071, 8.999999999999992895 ) ) ;
#2332 = ORIENTED_EDGE ( 'NONE', *, *, #22414, .T. ) ;
#2333 = CYLINDRICAL_SURFACE ( 'NONE', #9264, 0.5000000000000004441 ) ;
#2334 = CARTESIAN_POINT ( 'NONE',  ( 4.000000000000001776, 25.80624999877096926, 11.30940107675849760 ) ) ;
#2335 = CARTESIAN_POINT ( 'NONE',  ( -1.878215178125000939, -27.31562499938548427, 12.25316411605952283 ) ) ;
#2336 = EDGE_CURVE ( 'NONE', #9154, #24945, #19904, .T. ) ;
#2338 = ORIENTED_EDGE ( 'NONE', *, *, #8279, .F. ) ;
#2337 = CARTESIAN_POINT ( 'NONE',  ( -28.72825533807120024, 11.91206721063071505, 1.000000000000000000 ) ) ;
#2339 = EDGE_CURVE ( 'NONE', #3260, #21795, #3942, .T. ) ;
#2340 = EDGE_LOOP ( 'NONE', ( #22044, #21766, #23462, #9916 ) ) ;
#2341 = ORIENTED_EDGE ( 'NONE', *, *, #17195, .T. ) ;
#2342 = PRODUCT_DEFINITION_SHAPE ( 'NONE', 'NONE',  #17659 ) ;
#2343 = ORIENTED_EDGE ( 'NONE', *, *, #9994, .F. ) ;
#2344 = CARTESIAN_POINT ( 'NONE',  ( 26.49999999999999645, -0.5000000000000000000, 19.50000000000000000 ) ) ;
#2345 = EDGE_CURVE ( 'NONE', #22108, #19820, #19079, .T. ) ;
#2346 = CARTESIAN_POINT ( 'NONE',  ( 3.756430356250004543, 26.19062499938549138, 6.831223922626973533 ) ) ;
#2347 = FILL_AREA_STYLE ('',( #15819 ) ) ;
#2348 = CARTESIAN_POINT ( 'NONE',  ( 2.672651547586948120E-15, -13.33755215474602984, 4.078124999385480010 ) ) ;
#2349 = CARTESIAN_POINT ( 'NONE',  ( 3.756430356250003655, -8.999999999999992895, 0.7031249993854835623 ) ) ;
#2350 = SURFACE_STYLE_USAGE ( .BOTH. , #1962 ) ;
#2351 = CARTESIAN_POINT ( 'NONE',  ( -1.878215178124995832, 27.09062499938548640, 5.746835883940462963 ) ) ;
#2352 = CARTESIAN_POINT ( 'NONE',  ( -3.834746474454188013E-15, -27.36250000000000071, 4.999999999999992006 ) ) ;
#2353 = LINE ( 'NONE', #18303, #13470 ) ;
#2354 = CARTESIAN_POINT ( 'NONE',  ( -3.756430356249996994, 25.36562499938548498, 8.999999999999992895 ) ) ;
#2355 = DIRECTION ( 'NONE',  ( 0.000000000000000000, 1.000000000000000000, 0.000000000000000000 ) ) ;
#2356 = CARTESIAN_POINT ( 'NONE',  ( 22.19929630020171274, 20.18069571000422968, 12.74788474329069921 ) ) ;
#2357 = CARTESIAN_POINT ( 'NONE',  ( -22.32573188046936252, -21.65113613650319380, -6.500000000000000000 ) ) ;
#2358 = CARTESIAN_POINT ( 'NONE',  ( 3.999999999999996447, -29.21874999877096712, 8.999999999999992895 ) ) ;
#2359 = LINE ( 'NONE', #20530, #3564 ) ;
#2360 = CARTESIAN_POINT ( 'NONE',  ( 3.999999999999942268, -6.690598923241455331, 2.737500000000000266 ) ) ;
#2361 = CARTESIAN_POINT ( 'NONE',  ( -3.999999999999997335, 29.70624999877096784, 11.30940107675849404 ) ) ;
#2362 = DIRECTION ( 'NONE',  ( 0.000000000000000000, -0.000000000000000000, 1.000000000000000000 ) ) ;
#2363 = ORIENTED_EDGE ( 'NONE', *, *, #13575, .T. ) ;
#2364 = CARTESIAN_POINT ( 'NONE',  ( -20.92219106202066925, -23.01025686871623321, -2.750000000000000000 ) ) ;
#2366 = ORIENTED_EDGE ( 'NONE', *, *, #1130, .F. ) ;
#2365 = LINE ( 'NONE', #18198, #23752 ) ;
#2367 = EDGE_CURVE ( 'NONE', #6766, #2636, #12028, .T. ) ;
#2368 = ADVANCED_FACE ( 'NONE', ( #5645 ), #13625, .F. ) ;
#2369 = ORIENTED_EDGE ( 'NONE', *, *, #6160, .F. ) ;
#2370 = ORIENTED_EDGE ( 'NONE', *, *, #15295, .T. ) ;
#2371 = ORIENTED_EDGE ( 'NONE', *, *, #8349, .T. ) ;
#2372 = VERTEX_POINT ( 'NONE', #20006 ) ;
#2373 = ORIENTED_EDGE ( 'NONE', *, *, #8900, .F. ) ;
#2374 = DIRECTION ( 'NONE',  ( 1.000000000000000000, 0.000000000000000000, 0.000000000000000000 ) ) ;
#2375 = ORIENTED_EDGE ( 'NONE', *, *, #16611, .F. ) ;
#2376 = LINE ( 'NONE', #12040, #17207 ) ;
#2377 = CARTESIAN_POINT ( 'NONE',  ( 3.756430356250002323, 27.46562499938548640, 11.16877607737301403 ) ) ;
#2378 = EDGE_CURVE ( 'NONE', #930, #4422, #11895, .T. ) ;
#2379 = CARTESIAN_POINT ( 'NONE',  ( 3.735045420075836212E-15, -4.662447845253954171, 2.615624999385482319 ) ) ;
#2380 = CARTESIAN_POINT ( 'NONE',  ( 3.752267015613588906E-15, -4.381197846482986158, 1.406249998770964904 ) ) ;
#2381 = CARTESIAN_POINT ( 'NONE',  ( 22.02429405596265610, 16.71189930004383584, 8.999999999999992895 ) ) ;
#2382 = CARTESIAN_POINT ( 'NONE',  ( 19.68981756483611889, 21.20556709268809570, 12.99999999999999289 ) ) ;
#2383 = FILL_AREA_STYLE ('',( #6169 ) ) ;
#2384 = CARTESIAN_POINT ( 'NONE',  ( 3.756430356250002323, -11.16877607737301226, 1.003124999385480276 ) ) ;
#2385 = DIRECTION ( 'NONE',  ( 0.000000000000000000, -0.000000000000000000, 1.000000000000000000 ) ) ;
#2386 = CARTESIAN_POINT ( 'NONE',  ( -20.92219106202066925, -23.01025686871623321, -6.500000000000000000 ) ) ;
#2387 = CARTESIAN_POINT ( 'NONE',  ( 3.756430356250002323, -11.16877607737301403, 2.015624999385483118 ) ) ;
#2388 = CARTESIAN_POINT ( 'NONE',  ( -27.49048467073837898, 14.54246377227389075, 1.000000000000000000 ) ) ;
#2389 = CARTESIAN_POINT ( 'NONE',  ( 4.000000000000003553, 25.39374999877097494, 8.999999999999992895 ) ) ;
#2390 = VERTEX_POINT ( 'NONE', #14138 ) ;
#2391 = ORIENTED_EDGE ( 'NONE', *, *, #19509, .T. ) ;
#2392 = CARTESIAN_POINT ( 'NONE',  ( 1.878215178125001605, 27.87812499938548783, 12.25316411605952283 ) ) ;
#2393 = ORIENTED_EDGE ( 'NONE', *, *, #5656, .T. ) ;
#2394 = DIRECTION ( 'NONE',  ( 0.000000000000000000, -1.000000000000000000, 0.000000000000000000 ) ) ;
#2395 = ORIENTED_EDGE ( 'NONE', *, *, #10863, .T. ) ;
#2396 = CARTESIAN_POINT ( 'NONE',  ( -0.7500000000000000000, -2.999999999999999556, 17.69999999999999929 ) ) ;
#2397 = ORIENTED_EDGE ( 'NONE', *, *, #1567, .T. ) ;
#2398 = ORIENTED_EDGE ( 'NONE', *, *, #13996, .F. ) ;
#2399 = ADVANCED_FACE ( 'NONE', ( #5760 ), #19765, .T. ) ;
#2400 = CARTESIAN_POINT ( 'NONE',  ( 0.000000000000000000, 0.000000000000000000, 19.50000000000000000 ) ) ;
#2401 = CARTESIAN_POINT ( 'NONE',  ( 3.735045420075836212E-15, 27.05312499938548498, 4.662447845253954171 ) ) ;
#2402 = CARTESIAN_POINT ( 'NONE',  ( 1.878215178125006934, 29.26562499938549067, 5.746835883940462963 ) ) ;
#2403 = FACE_OUTER_BOUND ( 'NONE', #20273, .T. ) ;
#2404 = DIRECTION ( 'NONE',  ( 0.000000000000000000, 0.000000000000000000, -1.000000000000000000 ) ) ;
#2405 = CARTESIAN_POINT ( 'NONE',  ( -3.999999999999996447, 28.37500000000000355, 8.999999999999992895 ) ) ;
#2406 = EDGE_CURVE ( 'NONE', #13215, #25296, #17525, .T. ) ;
#2407 = CARTESIAN_POINT ( 'NONE',  ( 1.878215178125004048, 27.91562499938548569, 5.746835883940462963 ) ) ;
#2408 = CARTESIAN_POINT ( 'NONE',  ( -0.3342655765624286679, 38.86701176172695682, 3.376814578616960993 ) ) ;
#2409 = DIRECTION ( 'NONE',  ( -0.6374239897486843054, 0.7705132427757935831, 0.000000000000000000 ) ) ;
#2410 =( BOUNDED_CURVE ( )  B_SPLINE_CURVE ( 2, ( #20214, #4657, #22577, #12110, #22187, #20086, #2188, #619, #14473 ),
 .UNSPECIFIED., .F., .F. ) 
 B_SPLINE_CURVE_WITH_KNOTS ( ( 3, 2, 2, 2, 3 ),
 ( 0.3750000000000000000, 0.3833333333333333592, 0.4000000000000000222, 0.4166666666666666852, 0.4250000000000000444 ),
 .UNSPECIFIED. ) 
 CURVE ( )  GEOMETRIC_REPRESENTATION_ITEM ( )  RATIONAL_B_SPLINE_CURVE ( ( 0.9330127018922194093, 0.9330127018922194093, 1.000000000000000000, 0.8660254037844387076, 1.000000000000000000, 0.8660254037844387076, 1.000000000000000000, 0.9330127018922191873, 0.9330127018922194093 ) ) 
 REPRESENTATION_ITEM ( '' )  );
#2411 = CARTESIAN_POINT ( 'NONE',  ( 3.756430356249996105, -25.32812499938548356, 6.831223922626973533 ) ) ;
#2412 = AXIS2_PLACEMENT_3D ( 'NONE', #12844, #7087, #15076 ) ;
#2413 = DIRECTION ( 'NONE',  ( 1.000000000000000000, 0.000000000000000000, 0.000000000000000000 ) ) ;
#2414 = ORIENTED_EDGE ( 'NONE', *, *, #7302, .F. ) ;
#2415 = CARTESIAN_POINT ( 'NONE',  ( 2.000000000000000888, 29.81874999877096855, 12.46410161513774817 ) ) ;
#2416 = CARTESIAN_POINT ( 'NONE',  ( 19.46753356867312235, 19.46753356867304063, 12.99999999999999112 ) ) ;
#2418 = VERTEX_POINT ( 'NONE', #14656 ) ;
#2417 = CARTESIAN_POINT ( 'NONE',  ( 3.756430356250003211, 28.40312499938548640, 8.999999999999992895 ) ) ;
#2419 = ORIENTED_EDGE ( 'NONE', *, *, #19939, .T. ) ;
#2420 = DIRECTION ( 'NONE',  ( 0.000000000000000000, -0.000000000000000000, 1.000000000000000000 ) ) ;
#2421 =( BOUNDED_CURVE ( )  B_SPLINE_CURVE ( 2, ( #18067, #19869, #2236, #15975, #15710, #17798, #25764, #6276, #7845 ),
 .UNSPECIFIED., .F., .F. ) 
 B_SPLINE_CURVE_WITH_KNOTS ( ( 3, 2, 2, 2, 3 ),
 ( 0.1749999999999999889, 0.1833333333333333204, 0.2000000000000000111, 0.2166666666666666741, 0.2250000000000000056 ),
 .UNSPECIFIED. ) 
 CURVE ( )  GEOMETRIC_REPRESENTATION_ITEM ( )  RATIONAL_B_SPLINE_CURVE ( ( 0.9330127018922194093, 0.9330127018922194093, 1.000000000000000000, 0.8660254037844387076, 1.000000000000000000, 0.8660254037844387076, 1.000000000000000000, 0.9330127018922194093, 0.9330127018922194093 ) ) 
 REPRESENTATION_ITEM ( '' )  );
#2422 = CARTESIAN_POINT ( 'NONE',  ( 3.526711513754840599, 38.89679573513954125, 4.645898033750303746 ) ) ;
#2423 = CARTESIAN_POINT ( 'NONE',  ( -1.071796769724487230, 27.77634618820330559, 4.999999999999992006 ) ) ;
#2424 = AXIS2_PLACEMENT_3D ( 'NONE', #18763, #854, #12630 ) ;
#2425 = ORIENTED_EDGE ( 'NONE', *, *, #14687, .F. ) ;
#2426 = ORIENTED_EDGE ( 'NONE', *, *, #22750, .F. ) ;
#2427 = CARTESIAN_POINT ( 'NONE',  ( 1.878215178124995832, -26.30312499938548498, 5.746835883940462963 ) ) ;
#2428 = CARTESIAN_POINT ( 'NONE',  ( 3.756430356250003211, 27.39062499938548711, 8.999999999999992895 ) ) ;
#2429 = CARTESIAN_POINT ( 'NONE',  ( 0.000000000000000000, 0.000000000000000000, -6.500000000000000000 ) ) ;
#2430 = ADVANCED_FACE ( 'NONE', ( #20535 ), #12301, .F. ) ;
#2431 = CARTESIAN_POINT ( 'NONE',  ( 26.49999999999999645, -0.5000000000000000000, 19.50000000000000000 ) ) ;
#2432 = EDGE_CURVE ( 'NONE', #6934, #23536, #16699, .T. ) ;
#2433 = CIRCLE ( 'NONE', #22489, 31.10000000000000142 ) ;
#2434 = DIRECTION ( 'NONE',  ( 0.000000000000000000, 0.000000000000000000, 1.000000000000000000 ) ) ;
#2435 = DIRECTION ( 'NONE',  ( 0.000000000000000000, 0.000000000000000000, 1.000000000000000000 ) ) ;
#2436 = EDGE_CURVE ( 'NONE', #10602, #22990, #928, .T. ) ;
#2437 = CARTESIAN_POINT ( 'NONE',  ( 0.000000000000000000, 0.000000000000000000, 17.69999999999999929 ) ) ;
#2438 = CIRCLE ( 'NONE', #15040, 31.10000000000000142 ) ;
#2439 = CYLINDRICAL_SURFACE ( 'NONE', #24268, 31.10000000000000142 ) ;
#2440 = CARTESIAN_POINT ( 'NONE',  ( 19.46753356867312235, 19.46753356867304063, 12.99999999999999112 ) ) ;
#2441 = AXIS2_PLACEMENT_3D ( 'NONE', #4566, #24569, #2741 ) ;
#2442 = DIRECTION ( 'NONE',  ( 1.000000000000000000, 0.000000000000000000, 0.000000000000000000 ) ) ;
#2443 = CARTESIAN_POINT ( 'NONE',  ( 21.06742642710591440, 18.41122904914646341, 5.746835883940462963 ) ) ;
#2444 = CARTESIAN_POINT ( 'NONE',  ( 21.96892380712053239, 19.14049668237426616, 5.535898384862238508 ) ) ;
#2445 = CARTESIAN_POINT ( 'NONE',  ( -1.999999999999995781, 28.30000000000000071, 5.535898384862237620 ) ) ;
#2446 = FACE_OUTER_BOUND ( 'NONE', #24906, .T. ) ;
#2447 = CARTESIAN_POINT ( 'NONE',  ( 3.756430356250004099, 26.07812499938548356, 6.831223922626973533 ) ) ;
#2449 = ORIENTED_EDGE ( 'NONE', *, *, #113, .F. ) ;
#2448 = CARTESIAN_POINT ( 'NONE',  ( -0.5265545572341292502, 29.99647701088549923, 12.97381592328244082 ) ) ;
#2450 = CARTESIAN_POINT ( 'NONE',  ( 3.253724281355068545E-15, 25.50624999877097210, 4.999999999999992006 ) ) ;
#2451 = CARTESIAN_POINT ( 'NONE',  ( -7.248980000274416469, -30.24338421796776544, -6.500000000000000000 ) ) ;
#2452 = ORIENTED_EDGE ( 'NONE', *, *, #20965, .F. ) ;
#2453 = FACE_OUTER_BOUND ( 'NONE', #15004, .T. ) ;
#2454 = CARTESIAN_POINT ( 'NONE',  ( 3.469446951953614189E-15, 25.00000000000000000, 8.999999999999992895 ) ) ;
#2455 = CARTESIAN_POINT ( 'NONE',  ( 3.756430356249997882, -26.75312499938548427, 11.16877607737301226 ) ) ;
#2456 = ORIENTED_EDGE ( 'NONE', *, *, #23666, .F. ) ;
#2457 = AXIS2_PLACEMENT_3D ( 'NONE', #17604, #13291, #19546 ) ;
#2458 = ORIENTED_EDGE ( 'NONE', *, *, #23613, .T. ) ;
#2459 = CARTESIAN_POINT ( 'NONE',  ( -3.756430356250002323, -29.71562499938548640, 11.16877607737301226 ) ) ;
#2460 = ORIENTED_EDGE ( 'NONE', *, *, #7737, .F. ) ;
#2461 = ORIENTED_EDGE ( 'NONE', *, *, #25604, .T. ) ;
#2462 = CARTESIAN_POINT ( 'NONE',  ( -30.04913349766228592, -5.827558883615738594, 1.000000000000000000 ) ) ;
#2463 = CARTESIAN_POINT ( 'NONE',  ( -3.999999999999995559, 26.93124999877096926, 6.690598923241487306 ) ) ;
#2464 = VECTOR ( 'NONE', #11045, 1000.000000000000000 ) ;
#2465 = AXIS2_PLACEMENT_3D ( 'NONE', #20665, #18695, #2869 ) ;
#2466 = DIRECTION ( 'NONE',  ( 0.000000000000000000, 0.000000000000000000, -1.000000000000000000 ) ) ;
#2467 = CARTESIAN_POINT ( 'NONE',  ( 3.756430356250004099, -6.831223922626973533, 2.540624999385480809 ) ) ;
#2468 = PRESENTATION_STYLE_ASSIGNMENT (( #2350 ) ) ;
#2469 = EDGE_CURVE ( 'NONE', #486, #6625, #14572, .T. ) ;
#2470 = CARTESIAN_POINT ( 'NONE',  ( -3.756430356249996994, 29.52812499938548640, 8.999999999999992895 ) ) ;
#2471 = ADVANCED_FACE ( 'NONE', ( #8377 ), #10321, .F. ) ;
#2472 = DIRECTION ( 'NONE',  ( 0.000000000000000000, -0.000000000000000000, 1.000000000000000000 ) ) ;
#2473 = AXIS2_PLACEMENT_3D ( 'NONE', #12395, #8347, #16079 ) ;
#2474 = CARTESIAN_POINT ( 'NONE',  ( -9.133673601486680838, -29.72853858738275434, 1.000000000000000000 ) ) ;
#2475 = CARTESIAN_POINT ( 'NONE',  ( 3.735045420075836212E-15, 25.25312499938548427, 4.662447845253954171 ) ) ;
#2476 = DIRECTION ( 'NONE',  ( 0.000000000000000000, 0.000000000000000000, 1.000000000000000000 ) ) ;
#2477 = CARTESIAN_POINT ( 'NONE',  ( -9.610428525060479288, 29.57785765677940404, -6.500000000000000000 ) ) ;
#2478 = CARTESIAN_POINT ( 'NONE',  ( 1.500000000000001776, -7.499999999999993783, -6.938893903907228378E-15 ) ) ;
#2479 = CARTESIAN_POINT ( 'NONE',  ( -2.000000000000000888, -28.91874999877096997, 12.46410161513774817 ) ) ;
#2480 = EDGE_CURVE ( 'NONE', #15689, #16757, #16751, .T. ) ;
#2481 = B_SPLINE_CURVE_WITH_KNOTS ( 'NONE', 3,
 ( #5805, #23858, #25565, #19915, #7896, #11692, #9741, #13543, #7773, #17454, #17720, #19528, #1629, #21897 ),
 .UNSPECIFIED., .F., .F.,
 ( 4, 2, 2, 2, 2, 2, 4 ),
 ( 2.789812634828778690E-07, 0.0003151273862689746037, 0.0006299757912744662633, 0.0007873999937772171347, 0.0009448241962799682229, 0.001102248398782719203, 0.001259672601285470291 ),
 .UNSPECIFIED. ) ;
#2482 = CARTESIAN_POINT ( 'NONE',  ( -1.071796769724482123, 27.56740381056766864, 12.99999999999999645 ) ) ;
#2483 = VECTOR ( 'NONE', #15095, 1000.000000000000000 ) ;
#2484 = CARTESIAN_POINT ( 'NONE',  ( -1.999999999999998224, 28.00000000000000000, 12.46410161513774639 ) ) ;
#2485 = CARTESIAN_POINT ( 'NONE',  ( -30.45149776762733751, -6.317933499823126908, 1.000000000000000000 ) ) ;
#2486 = CARTESIAN_POINT ( 'NONE',  ( 20.46970022635141362, 14.98507572364578699, 8.999999999999992895 ) ) ;
#2487 = ORIENTED_EDGE ( 'NONE', *, *, #2756, .T. ) ;
#2488 = CARTESIAN_POINT ( 'NONE',  ( -5.840899737312981621, 34.50000000000000000, 7.627451181685283466 ) ) ;
#2490 = ORIENTED_EDGE ( 'NONE', *, *, #11535, .T. ) ;
#2489 = CARTESIAN_POINT ( 'NONE',  ( 27.10000000000000142, 3.318792825689327485E-15, 1.000000000000000000 ) ) ;
#2491 = EDGE_LOOP ( 'NONE', ( #11578, #21763, #25653, #7166 ) ) ;
#2492 = AXIS2_PLACEMENT_3D ( 'NONE', #24578, #787, #8762 ) ;
#2493 = ORIENTED_EDGE ( 'NONE', *, *, #3693, .F. ) ;
#2494 = VERTEX_POINT ( 'NONE', #14405 ) ;
#2495 = EDGE_LOOP ( 'NONE', ( #10958, #9083, #13510, #24271 ) ) ;
#2496 = ORIENTED_EDGE ( 'NONE', *, *, #10513, .T. ) ;
#2497 = DIRECTION ( 'NONE',  ( 1.000000000000000000, 0.000000000000000000, 0.000000000000000000 ) ) ;
#2498 = CIRCLE ( 'NONE', #17120, 0.4999999999999996669 ) ;
#2499 = AXIS2_PLACEMENT_3D ( 'NONE', #2842, #1023, #7022 ) ;
#2500 = ORIENTED_EDGE ( 'NONE', *, *, #20767, .T. ) ;
#2501 = CYLINDRICAL_SURFACE ( 'NONE', #14849, 0.5000000000000004441 ) ;
#2502 = CARTESIAN_POINT ( 'NONE',  ( -1.878215178124998497, 26.45312499938548711, 12.25316411605951927 ) ) ;
#2503 = AXIS2_PLACEMENT_3D ( 'NONE', #6228, #11733, #22193 ) ;
#2504 = AXIS2_PLACEMENT_3D ( 'NONE', #11262, #1081, #15331 ) ;
#2505 = EDGE_CURVE ( 'NONE', #184, #12340, #22364, .T. ) ;
#2506 = CARTESIAN_POINT ( 'NONE',  ( 3.756430356250004099, -6.831223922626973533, 2.540624999385480809 ) ) ;
#2507 = DIRECTION ( 'NONE',  ( 0.000000000000000000, -0.000000000000000000, -1.000000000000000000 ) ) ;
#2508 = CARTESIAN_POINT ( 'NONE',  ( 18.49305203628493288, 18.49305203628486183, 4.662447845253954171 ) ) ;
#2509 = CARTESIAN_POINT ( 'NONE',  ( -26.25859848311247902, 16.66421332384710752, -6.500000000000000000 ) ) ;
#2510 = EDGE_CURVE ( 'NONE', #6672, #9003, #19601, .T. ) ;
#2511 = CARTESIAN_POINT ( 'NONE',  ( -19.82388608118395013, 23.96296185032730364, 1.000000000000000000 ) ) ;
#2512 = CARTESIAN_POINT ( 'NONE',  ( 1.878215178125004048, -5.746835883940462963, 2.015624999385484450 ) ) ;
#2513 = CARTESIAN_POINT ( 'NONE',  ( -1.999999999999995781, 27.79374999877096997, 5.535898384862237620 ) ) ;
#2514 = CARTESIAN_POINT ( 'NONE',  ( -4.393401135981330086, -30.78811501957140351, -2.750000000000000000 ) ) ;
#2515 = AXIS2_PLACEMENT_3D ( 'NONE', #13737, #15318, #1852 ) ;
#2516 = CARTESIAN_POINT ( 'NONE',  ( -3.756430356249996105, -6.831223922626973533, 0.8906249993854813418 ) ) ;
#2517 = CARTESIAN_POINT ( 'NONE',  ( 16.64794527869176122, 19.47637240343788179, 5.535898384862237620 ) ) ;
#2518 = DIRECTION ( 'NONE',  ( -0.000000000000000000, -0.000000000000000000, -1.000000000000000000 ) ) ;
#2519 = ORIENTED_EDGE ( 'NONE', *, *, #23305, .T. ) ;
#2520 = ORIENTED_EDGE ( 'NONE', *, *, #16662, .F. ) ;
#2521 = CARTESIAN_POINT ( 'NONE',  ( 3.756430356250000546, 28.36562499938549564, 11.16877607737301226 ) ) ;
#2522 = AXIS2_PLACEMENT_3D ( 'NONE', #16518, #4990, #16632 ) ;
#2523 = ADVANCED_FACE ( 'NONE', ( #6808 ), #24722, .T. ) ;
#2524 = ORIENTED_EDGE ( 'NONE', *, *, #13156, .F. ) ;
#2525 = CARTESIAN_POINT ( 'NONE',  ( -3.918623196469422698, 34.50000000000000000, 13.54361004533748059 ) ) ;
#2526 = ORIENTED_EDGE ( 'NONE', *, *, #4172, .F. ) ;
#2527 = CARTESIAN_POINT ( 'NONE',  ( -1.999999999999998224, 28.30000000000000426, 5.535898384862237620 ) ) ;
#2528 = EDGE_LOOP ( 'NONE', ( #6641, #17739, #11163 ) ) ;
#2529 = DIRECTION ( 'NONE',  ( 0.000000000000000000, 0.000000000000000000, 1.000000000000000000 ) ) ;
#2530 = DIRECTION ( 'NONE',  ( 1.000000000000000000, 0.000000000000000000, 0.000000000000000000 ) ) ;
#2531 = AXIS2_PLACEMENT_3D ( 'NONE', #17826, #12196, #9725 ) ;
#2532 = ORIENTED_EDGE ( 'NONE', *, *, #3191, .F. ) ;
#2533 = LINE ( 'NONE', #10122, #10134 ) ;
#2534 = CARTESIAN_POINT ( 'NONE',  ( 1.878215178125000939, 27.31562499938548427, 12.25316411605952283 ) ) ;
#2535 = CARTESIAN_POINT ( 'NONE',  ( 1.071796769724492338, 28.95759618943233704, 12.99999999999999467 ) ) ;
#2536 = AXIS2_PLACEMENT_3D ( 'NONE', #15735, #21999, #13642 ) ;
#2537 = DIRECTION ( 'NONE',  ( 0.000000000000000000, 0.000000000000000000, 1.000000000000000000 ) ) ;
#2538 = CARTESIAN_POINT ( 'NONE',  ( 21.28941499438225904, 22.67092431280586240, -6.500000000000000000 ) ) ;
#2539 = CARTESIAN_POINT ( 'NONE',  ( 2.000000000000003553, 29.12500000000000355, 5.535898384862238508 ) ) ;
#2540 = CIRCLE ( 'NONE', #5879, 31.10000000000000142 ) ;
#2541 = VECTOR ( 'NONE', #10189, 1000.000000000000000 ) ;
#2542 = CARTESIAN_POINT ( 'NONE',  ( 3.756430356250003655, 28.74062499938548498, 8.999999999999992895 ) ) ;
#2543 = EDGE_CURVE ( 'NONE', #23953, #20546, #6287, .T. ) ;
#2544 = CARTESIAN_POINT ( 'NONE',  ( 19.23778763078571430, 16.58159025282627397, 5.746835883940462963 ) ) ;
#2545 = CARTESIAN_POINT ( 'NONE',  ( -3.999999999999996447, -8.999999999999992895, 2.024999999999999023 ) ) ;
#2546 = PRODUCT ( 'indicator hand', 'indicator hand', '', ( #13281 ) ) ;
#2547 = CARTESIAN_POINT ( 'NONE',  ( 4.006172263299091013E-15, 25.50624999877097920, 4.381197846482986158 ) ) ;
#2548 = CARTESIAN_POINT ( 'NONE',  ( -3.999999999999995559, 29.18124999877096926, 6.690598923241487306 ) ) ;
#2549 = AXIS2_PLACEMENT_3D ( 'NONE', #19963, #2067, #16069 ) ;
#2550 = CARTESIAN_POINT ( 'NONE',  ( -2.672651547586948120E-15, -28.62812499938548783, 13.33755215474603162 ) ) ;
#2551 = VECTOR ( 'NONE', #23517, 1000.000000000000000 ) ;
#2552 = CARTESIAN_POINT ( 'NONE',  ( 5.621027209102163802, 38.71721868403345468, 10.35826165063589777 ) ) ;
#2553 = VERTEX_POINT ( 'NONE', #12420 ) ;
#2554 = CARTESIAN_POINT ( 'NONE',  ( -3.756430356249997882, 25.96562499938548640, 11.16877607737301226 ) ) ;
#2555 = CARTESIAN_POINT ( 'NONE',  ( 1.999999999999995781, -28.30000000000000071, 5.535898384862237620 ) ) ;
#2557 = ORIENTED_EDGE ( 'NONE', *, *, #11543, .T. ) ;
#2556 = CARTESIAN_POINT ( 'NONE',  ( -3.756430356249997882, 27.72812499938548569, 8.999999999999992895 ) ) ;
#2558 = ORIENTED_EDGE ( 'NONE', *, *, #8063, .T. ) ;
#2559 = CARTESIAN_POINT ( 'NONE',  ( 23.64116323484238080, 20.20656826142275264, -6.500000000000000000 ) ) ;
#2560 = VECTOR ( 'NONE', #24669, 1000.000000000000000 ) ;
#2561 = DIRECTION ( 'NONE',  ( -0.000000000000000000, 1.000000000000000000, -0.000000000000000000 ) ) ;
#2562 = CARTESIAN_POINT ( 'NONE',  ( -25.99519186311192342, -0.5000000000000000000, 20.00000000000000000 ) ) ;
#2563 = ORIENTED_EDGE ( 'NONE', *, *, #16767, .F. ) ;
#2564 = VERTEX_POINT ( 'NONE', #22638 ) ;
#2565 = CARTESIAN_POINT ( 'NONE',  ( -2.672651547586948120E-15, -27.84062499938548640, 13.33755215474603162 ) ) ;
#2566 = CARTESIAN_POINT ( 'NONE',  ( 3.756430356250003211, 26.94062499938548783, 8.999999999999992895 ) ) ;
#2567 = CARTESIAN_POINT ( 'NONE',  ( -4.000000000000003553, -29.03124999877096712, 6.690598923241489970 ) ) ;
#2568 = AXIS2_PLACEMENT_3D ( 'NONE', #15890, #11564, #5947 ) ;
#2569 = DIRECTION ( 'NONE',  ( -0.000000000000000000, -1.000000000000000000, -0.000000000000000000 ) ) ;
#2570 = VECTOR ( 'NONE', #209, 1000.000000000000000 ) ;
#2571 = CIRCLE ( 'NONE', #5914, 26.00000000000000355 ) ;
#2572 = CARTESIAN_POINT ( 'NONE',  ( 20.42212772327495784, 20.42212772327488679, 12.99999999999999289 ) ) ;
#2573 =( NAMED_UNIT ( * ) SI_UNIT ( $, .STERADIAN. ) SOLID_ANGLE_UNIT ( ) );
#2574 =( BOUNDED_CURVE ( )  B_SPLINE_CURVE ( 2, ( #15669, #5847, #2195, #15785, #8200, #228, #23636, #25725, #5714 ),
 .UNSPECIFIED., .F., .F. ) 
 B_SPLINE_CURVE_WITH_KNOTS ( ( 3, 2, 2, 2, 3 ),
 ( 0.6250000000000000000, 0.6333333333333333037, 0.6500000000000000222, 0.6666666666666666297, 0.6750000000000000444 ),
 .UNSPECIFIED. ) 
 CURVE ( )  GEOMETRIC_REPRESENTATION_ITEM ( )  RATIONAL_B_SPLINE_CURVE ( ( 0.9330127018922194093, 0.9330127018922194093, 1.000000000000000000, 0.8660254037844387076, 1.000000000000000000, 0.8660254037844387076, 1.000000000000000000, 0.9330127018922189652, 0.9330127018922194093 ) ) 
 REPRESENTATION_ITEM ( '' )  );
#2575 = CARTESIAN_POINT ( 'NONE',  ( -3.834746474454188013E-15, -28.26249999999999929, 4.999999999999992006 ) ) ;
#2576 = VECTOR ( 'NONE', #24031, 1000.000000000000000 ) ;
#2577 = DIRECTION ( 'NONE',  ( 0.000000000000000000, 0.000000000000000000, 1.000000000000000000 ) ) ;
#2578 = EDGE_CURVE ( 'NONE', #18387, #14523, #17115, .T. ) ;
#2579 = CARTESIAN_POINT ( 'NONE',  ( 25.45105997952912702, -17.87326343783951899, -6.500000000000000000 ) ) ;
#2580 = DIRECTION ( 'NONE',  ( -0.7705132427757840352, 0.6374239897486960738, 0.000000000000000000 ) ) ;
#2581 = CARTESIAN_POINT ( 'NONE',  ( 17.82786595466764012, 20.48406333262694190, 5.746835883940462963 ) ) ;
#2582 = CARTESIAN_POINT ( 'NONE',  ( 22.34899370200829338, 16.69213945251583908, 11.30940107675849760 ) ) ;
#2583 = CARTESIAN_POINT ( 'NONE',  ( -1.999999999999998224, 28.44999999999999929, 12.46410161513774639 ) ) ;
#2584 = DIRECTION ( 'NONE',  ( 0.000000000000000000, 0.000000000000000000, 1.000000000000000000 ) ) ;
#2585 =( BOUNDED_CURVE ( )  B_SPLINE_CURVE ( 2, ( #18288, #18174, #16471, #4543, #12523, #18044, #6510, #6633, #18418 ),
 .UNSPECIFIED., .F., .F. ) 
 B_SPLINE_CURVE_WITH_KNOTS ( ( 3, 2, 2, 2, 3 ),
 ( 0.2250000000000000056, 0.2333333333333333370, 0.2500000000000000000, 0.2666666666666666630, 0.2750000000000000222 ),
 .UNSPECIFIED. ) 
 CURVE ( )  GEOMETRIC_REPRESENTATION_ITEM ( )  RATIONAL_B_SPLINE_CURVE ( ( 0.9330127018922194093, 0.9330127018922194093, 1.000000000000000000, 0.8660254037844387076, 1.000000000000000000, 0.8660254037844387076, 1.000000000000000000, 0.9330127018922191873, 0.9330127018922194093 ) ) 
 REPRESENTATION_ITEM ( '' )  );
#2586 = CARTESIAN_POINT ( 'NONE',  ( -1.878215178124998497, 29.60312499938548569, 12.25316411605951927 ) ) ;
#2589 = EDGE_CURVE ( 'NONE', #13396, #21005, #14278, .T. ) ;
#2588 = ORIENTED_EDGE ( 'NONE', *, *, #13785, .F. ) ;
#2587 = CARTESIAN_POINT ( 'NONE',  ( -1.039771317798496408, 29.98307469845295969, 12.87134967428165666 ) ) ;
#2590 = AXIS2_PLACEMENT_3D ( 'NONE', #24800, #12151, #265 ) ;
#2591 = CARTESIAN_POINT ( 'NONE',  ( 15.30652457243565046, 20.61891932835433394, 11.16877607737301048 ) ) ;
#2592 = CARTESIAN_POINT ( 'NONE',  ( 20.41770830676159676, 17.58928118201533408, 5.535898384862238508 ) ) ;
#2593 = ORIENTED_EDGE ( 'NONE', *, *, #1215, .T. ) ;
#2594 = CARTESIAN_POINT ( 'NONE',  ( 25.99307600111999150, 0.5999999999999998668, 19.00000000000000000 ) ) ;
#2595 = CARTESIAN_POINT ( 'NONE',  ( -1.452785157361201396, 31.03863125411927371, -6.500000000000000000 ) ) ;
#2596 = CARTESIAN_POINT ( 'NONE',  ( -3.756430356250003655, -25.59062499938548285, 8.999999999999992895 ) ) ;
#2598 = ORIENTED_EDGE ( 'NONE', *, *, #22688, .T. ) ;
#2597 = DIRECTION ( 'NONE',  ( 0.000000000000000000, 0.000000000000000000, 1.000000000000000000 ) ) ;
#2599 = EDGE_CURVE ( 'NONE', #5942, #4195, #2627, .T. ) ;
#2600 = CIRCLE ( 'NONE', #8027, 31.10000000000000142 ) ;
#2601 = CYLINDRICAL_SURFACE ( 'NONE', #12898, 4.000000000000000000 ) ;
#2602 = VECTOR ( 'NONE', #11902, 1000.000000000000000 ) ;
#2603 = ORIENTED_EDGE ( 'NONE', *, *, #4982, .T. ) ;
#2604 = CARTESIAN_POINT ( 'NONE',  ( 3.756430356249997882, -26.75312499938548427, 11.16877607737301226 ) ) ;
#2605 = EDGE_LOOP ( 'NONE', ( #20644, #21893 ) ) ;
#2606 = ADVANCED_FACE ( 'NONE', ( #2874 ), #8518, .T. ) ;
#2607 = VERTEX_POINT ( 'NONE', #16615 ) ;
#2608 = DIRECTION ( 'NONE',  ( -0.000000000000000000, -0.000000000000000000, 1.000000000000000000 ) ) ;
#2609 = CYLINDRICAL_SURFACE ( 'NONE', #23897, 0.5000000000000004441 ) ;
#2610 = LINE ( 'NONE', #10434, #6412 ) ;
#2611 = VECTOR ( 'NONE', #3149, 1000.000000000000000 ) ;
#2612 = CARTESIAN_POINT ( 'NONE',  ( 1.878215178125000939, -12.25316411605952283, 1.978124999385485250 ) ) ;
#2613 = LINE ( 'NONE', #12931, #18471 ) ;
#2614 = CARTESIAN_POINT ( 'NONE',  ( 3.735045420075836212E-15, 25.25312499938548783, 4.662447845253954171 ) ) ;
#2615 = VECTOR ( 'NONE', #13942, 1000.000000000000000 ) ;
#2616 = CARTESIAN_POINT ( 'NONE',  ( 20.46190248058575634, 20.46190248058568173, 12.99999999999999289 ) ) ;
#2617 = DIRECTION ( 'NONE',  ( 1.000000000000000000, 0.000000000000000000, 0.000000000000000000 ) ) ;
#2618 = CARTESIAN_POINT ( 'NONE',  ( 3.756430356250003655, 25.14062499938548356, 8.999999999999992895 ) ) ;
#2619 = CARTESIAN_POINT ( 'NONE',  ( -0.7500000000000001110, 0.000000000000000000, 17.69999999999999929 ) ) ;
#2620 = CARTESIAN_POINT ( 'NONE',  ( -3.999999999999953371, -6.690598923241463325, 1.031249998770966458 ) ) ;
#2621 = CARTESIAN_POINT ( 'NONE',  ( -1.878215178125004048, -26.22812499938548569, 5.746835883940462963 ) ) ;
#2622 = CARTESIAN_POINT ( 'NONE',  ( -1.071796769724485232, 27.38259618943233775, 4.999999999999992006 ) ) ;
#2623 = CARTESIAN_POINT ( 'NONE',  ( 4.000000000000003553, -8.999999999999992895, 3.149999999999999911 ) ) ;
#2624 = CARTESIAN_POINT ( 'NONE',  ( -3.397863563849436108, 30.85476721088031482, -6.500000000000000000 ) ) ;
#2625 = CARTESIAN_POINT ( 'NONE',  ( -1.071796769724487230, 27.83259618943233704, 4.999999999999992006 ) ) ;
#2626 = ORIENTED_EDGE ( 'NONE', *, *, #846, .F. ) ;
#2627 = LINE ( 'NONE', #18454, #20438 ) ;
#2629 = ORIENTED_EDGE ( 'NONE', *, *, #8813, .F. ) ;
#2628 = DIRECTION ( 'NONE',  ( 0.000000000000000000, 0.000000000000000000, -1.000000000000000000 ) ) ;
#2630 = ADVANCED_FACE ( 'NONE', ( #4724 ), #21062, .T. ) ;
#2631 = ORIENTED_EDGE ( 'NONE', *, *, #16128, .T. ) ;
#2632 = ORIENTED_EDGE ( 'NONE', *, *, #20451, .F. ) ;
#2633 = ORIENTED_EDGE ( 'NONE', *, *, #25293, .T. ) ;
#2634 = EDGE_CURVE ( 'NONE', #15214, #10104, #12507, .T. ) ;
#2635 = ORIENTED_EDGE ( 'NONE', *, *, #1504, .T. ) ;
#2636 = VERTEX_POINT ( 'NONE', #17392 ) ;
#2637 = CYLINDRICAL_SURFACE ( 'NONE', #21391, 31.10000000000000142 ) ;
#2638 = EDGE_CURVE ( 'NONE', #10597, #19004, #4581, .T. ) ;
#2639 = AXIS2_PLACEMENT_3D ( 'NONE', #5729, #9666, #17649 ) ;
#2640 = ORIENTED_EDGE ( 'NONE', *, *, #8385, .T. ) ;
#2641 = DIRECTION ( 'NONE',  ( 0.000000000000000000, 0.000000000000000000, -1.000000000000000000 ) ) ;
#2642 = CARTESIAN_POINT ( 'NONE',  ( -1.878215178124998497, 28.25312499938548427, 12.25316411605951927 ) ) ;
#2643 = VECTOR ( 'NONE', #17666, 1000.000000000000000 ) ;
#2644 = CARTESIAN_POINT ( 'NONE',  ( -1.878215178124995832, -5.746835883940462963, 3.103124999385483029 ) ) ;
#2645 = CARTESIAN_POINT ( 'NONE',  ( 22.02202058170775345, 19.36582320374829891, 5.746835883940462963 ) ) ;
#2646 = FACE_OUTER_BOUND ( 'NONE', #4165, .T. ) ;
#2647 = AXIS2_PLACEMENT_3D ( 'NONE', #15781, #24015, #19563 ) ;
#2648 = CARTESIAN_POINT ( 'NONE',  ( -26.00000000000000355, -1.592040838891558504E-15, 20.00000599999999906 ) ) ;
#2649 = CARTESIAN_POINT ( 'NONE',  ( 1.878215178125004048, -5.746835883940462963, 2.915624999385482585 ) ) ;
#2650 = DIRECTION ( 'NONE',  ( 0.9048270524660262382, 0.4257792915650585042, 0.000000000000000000 ) ) ;
#2651 = CARTESIAN_POINT ( 'NONE',  ( 2.000000000000003997, -5.535898384862238508, 3.224999999999998757 ) ) ;
#2652 = CARTESIAN_POINT ( 'NONE',  ( -1.071796769724488785, 28.86115380933863861, 12.99999999999999289 ) ) ;
#2653 = CARTESIAN_POINT ( 'NONE',  ( -2.000000000000003997, -25.46874999877096712, 5.535898384862238508 ) ) ;
#2654 = CARTESIAN_POINT ( 'NONE',  ( 3.756430356250003211, -6.831223922626973533, 2.540624999385480809 ) ) ;
#2655 = CARTESIAN_POINT ( 'NONE',  ( 3.469446951953614189E-15, -8.999999999999992895, 0.000000000000000000 ) ) ;
#2656 = ORIENTED_EDGE ( 'NONE', *, *, #13667, .T. ) ;
#2657 = EDGE_LOOP ( 'NONE', ( #4903, #21039, #15568, #5873 ) ) ;
#2658 = CARTESIAN_POINT ( 'NONE',  ( -3.756430356249996549, 26.82812499938549067, 8.999999999999992895 ) ) ;
#2659 = ORIENTED_EDGE ( 'NONE', *, *, #5988, .T. ) ;
#2660 = CARTESIAN_POINT ( 'NONE',  ( 1.952785157361650370, 31.03863125411924528, 1.000000000000000000 ) ) ;
#2661 = STYLED_ITEM ( 'NONE', ( #20909 ), #1303 ) ;
#2662 = EDGE_LOOP ( 'NONE', ( #13155, #20391, #24862, #18260 ) ) ;
#2663 = FACE_OUTER_BOUND ( 'NONE', #9440, .T. ) ;
#2664 = EDGE_LOOP ( 'NONE', ( #12172, #8183, #18204, #6376 ) ) ;
#2665 = CYLINDRICAL_SURFACE ( 'NONE', #7591, 0.5000000000000004441 ) ;
#2666 = EDGE_CURVE ( 'NONE', #18977, #7736, #18968, .T. ) ;
#2667 = VECTOR ( 'NONE', #3651, 1000.000000000000000 ) ;
#2668 = DIRECTION ( 'NONE',  ( 1.000000000000000000, 0.000000000000000000, 0.000000000000000000 ) ) ;
#2669 = ORIENTED_EDGE ( 'NONE', *, *, #9832, .T. ) ;
#2670 = DIRECTION ( 'NONE',  ( 0.000000000000000000, 0.000000000000000000, 1.000000000000000000 ) ) ;
#2671 = CARTESIAN_POINT ( 'NONE',  ( 2.000000000000000888, 25.37500000000000000, 12.46410161513774817 ) ) ;
#2672 = CYLINDRICAL_SURFACE ( 'NONE', #6392, 0.5000000000000004441 ) ;
#2673 = CARTESIAN_POINT ( 'NONE',  ( -31.10000000000000142, 3.257552089140643357E-13, 1.000000000000000000 ) ) ;
#2674 = DIRECTION ( 'NONE',  ( 0.000000000000000000, 0.000000000000000000, -1.000000000000000000 ) ) ;
#2675 = CARTESIAN_POINT ( 'NONE',  ( 18.09530447186750024, 18.09530447186743629, 13.33755215474602984 ) ) ;
#2676 =( GEOMETRIC_REPRESENTATION_CONTEXT ( 3 ) GLOBAL_UNCERTAINTY_ASSIGNED_CONTEXT ( ( #12808 ) ) GLOBAL_UNIT_ASSIGNED_CONTEXT ( ( #3892, #25726, #22442 ) ) REPRESENTATION_CONTEXT ( 'NONE', 'WORKASPACE' ) );
#2677 = CARTESIAN_POINT ( 'NONE',  ( 3.756430356250003655, 28.29062499938548569, 8.999999999999992895 ) ) ;
#2678 = CARTESIAN_POINT ( 'NONE',  ( 10.98232076577212624, -29.09636799667083196, 1.000000000000000000 ) ) ;
#2679 = DIRECTION ( 'NONE',  ( 0.000000000000000000, 0.000000000000000000, 1.000000000000000000 ) ) ;
#2680 = CARTESIAN_POINT ( 'NONE',  ( 2.000000000000000000, 26.21874999877097423, 12.46410161513774817 ) ) ;
#2681 = DIRECTION ( 'NONE',  ( 0.000000000000000000, -0.000000000000000000, -1.000000000000000000 ) ) ;
#2682 = CARTESIAN_POINT ( 'NONE',  ( -1.878215178125004048, -27.91562499938548569, 5.746835883940462963 ) ) ;
#2683 = CARTESIAN_POINT ( 'NONE',  ( 5.451523067058389849, 38.86679461760645182, 10.41960775444208842 ) ) ;
#2684 = EDGE_LOOP ( 'NONE', ( #23658, #14103, #22454, #9448 ) ) ;
#2685 = CARTESIAN_POINT ( 'NONE',  ( 2.672651547586948120E-15, 26.04062499938548925, 13.33755215474602984 ) ) ;
#2686 = CARTESIAN_POINT ( 'NONE',  ( 19.62663259444009611, 19.62663259444001085, 4.999999999999992006 ) ) ;
#2688 = ORIENTED_EDGE ( 'NONE', *, *, #22471, .T. ) ;
#2687 = FACE_OUTER_BOUND ( 'NONE', #1056, .T. ) ;
#2689 = EDGE_CURVE ( 'NONE', #5115, #24168, #16292, .T. ) ;
#2690 = VERTEX_POINT ( 'NONE', #12951 ) ;
#2691 = CYLINDRICAL_SURFACE ( 'NONE', #4972, 6.000000000000000888 ) ;
#2692 = EDGE_CURVE ( 'NONE', #22640, #11825, #5350, .T. ) ;
#2693 = CARTESIAN_POINT ( 'NONE',  ( -3.999999999999996447, -8.999999999999992895, 4.218749998770966236 ) ) ;
#2694 = ORIENTED_EDGE ( 'NONE', *, *, #6490, .F. ) ;
#2695 = CARTESIAN_POINT ( 'NONE',  ( -1.878215178125004048, -28.02812499938548640, 5.746835883940462963 ) ) ;
#2696 = CARTESIAN_POINT ( 'NONE',  ( 1.071796769724494558, 25.99240381056766580, 4.999999999999992895 ) ) ;
#2697 = ADVANCED_FACE ( 'NONE', ( #1307 ), #1560, .T. ) ;
#2698 = DIRECTION ( 'NONE',  ( 0.000000000000000000, 0.000000000000000000, 1.000000000000000000 ) ) ;
#2699 = CARTESIAN_POINT ( 'NONE',  ( -3.756430356249998326, 25.85312499938549635, 11.16877607737301226 ) ) ;
#2700 = EDGE_CURVE ( 'NONE', #19352, #12340, #24642, .T. ) ;
#2701 = DIRECTION ( 'NONE',  ( 0.000000000000000000, 0.000000000000000000, -1.000000000000000000 ) ) ;
#2702 = FACE_OUTER_BOUND ( 'NONE', #19595, .T. ) ;
#2703 = CYLINDRICAL_SURFACE ( 'NONE', #20515, 0.5000000000000004441 ) ;
#2704 = CARTESIAN_POINT ( 'NONE',  ( 1.878215178125004048, 25.21562499938548285, 5.746835883940462963 ) ) ;
#2705 = CARTESIAN_POINT ( 'NONE',  ( 30.85476721088027929, 3.897863563849760737, -6.500000000000000000 ) ) ;
#2706 = CARTESIAN_POINT ( 'NONE',  ( 17.16267987305034382, 22.47507462896901842, 6.831223922626973533 ) ) ;
#2707 = CARTESIAN_POINT ( 'NONE',  ( 20.51285331117640709, 15.20045855525759393, 8.999999999999992895 ) ) ;
#2708 = PLANE ( 'NONE',  #24311 ) ;
#2709 = DIRECTION ( 'NONE',  ( 1.000000000000000000, 0.000000000000000000, 0.000000000000000000 ) ) ;
#2710 = CARTESIAN_POINT ( 'NONE',  ( -3.756430356249996994, 29.07812499938548356, 8.999999999999992895 ) ) ;
#2712 = ORIENTED_EDGE ( 'NONE', *, *, #7114, .T. ) ;
#2711 = FACE_OUTER_BOUND ( 'NONE', #8416, .T. ) ;
#2713 = CARTESIAN_POINT ( 'NONE',  ( 16.87327180006579752, 19.52946917802510285, 5.746835883940462963 ) ) ;
#2714 = CARTESIAN_POINT ( 'NONE',  ( 20.42212772327495784, 20.42212772327488679, 12.99999999999999289 ) ) ;
#2715 = ORIENTED_EDGE ( 'NONE', *, *, #900, .F. ) ;
#2716 = CARTESIAN_POINT ( 'NONE',  ( 3.834746474454188013E-15, 25.95624999877096428, 4.999999999999992006 ) ) ;
#2717 = CARTESIAN_POINT ( 'NONE',  ( -1.999999999999995781, 26.89374999877097139, 5.535898384862237620 ) ) ;
#2718 = CARTESIAN_POINT ( 'NONE',  ( 3.756430356249997882, -27.65312499938548640, 11.16877607737301226 ) ) ;
#2720 = ORIENTED_EDGE ( 'NONE', *, *, #22691, .T. ) ;
#2719 = DIRECTION ( 'NONE',  ( 0.000000000000000000, 0.000000000000000000, 1.000000000000000000 ) ) ;
#2721 = DIRECTION ( 'NONE',  ( 1.000000000000000000, 0.000000000000000000, 0.000000000000000000 ) ) ;
#2722 = VERTEX_POINT ( 'NONE', #22885 ) ;
#2723 = CARTESIAN_POINT ( 'NONE',  ( 3.756430356249996994, -26.26562499938548711, 8.999999999999992895 ) ) ;
#2724 = ORIENTED_EDGE ( 'NONE', *, *, #7392, .T. ) ;
#2725 = ORIENTED_EDGE ( 'NONE', *, *, #7581, .F. ) ;
#2726 = CARTESIAN_POINT ( 'NONE',  ( -8.831537335106614961E-15, -27.53124999877097068, 12.99999999999999112 ) ) ;
#2727 = DIRECTION ( 'NONE',  ( 0.000000000000000000, 0.000000000000000000, -1.000000000000000000 ) ) ;
#2728 = EDGE_CURVE ( 'NONE', #16373, #19798, #11228, .T. ) ;
#2729 = AXIS2_PLACEMENT_3D ( 'NONE', #24331, #662, #24455 ) ;
#2730 = CARTESIAN_POINT ( 'NONE',  ( 1.071796769724498999, 27.60759618943233207, 12.99999999999998757 ) ) ;
#2731 =( BOUNDED_CURVE ( )  B_SPLINE_CURVE ( 2, ( #15582, #17410, #19227, #9428, #25373, #9546, #15446 ),
 .UNSPECIFIED., .F., .F. ) 
 B_SPLINE_CURVE_WITH_KNOTS ( ( 3, 2, 2, 3 ),
 ( 0.7500000000000000000, 0.7666666666666667185, 0.7833333333333332149, 0.7999999999999999334 ),
 .UNSPECIFIED. ) 
 CURVE ( )  GEOMETRIC_REPRESENTATION_ITEM ( )  RATIONAL_B_SPLINE_CURVE ( ( 1.000000000000000000, 0.8660254037844387076, 1.000000000000000000, 0.8660254037844387076, 1.000000000000000000, 0.8660254037844395958, 0.9999999999999991118 ) ) 
 REPRESENTATION_ITEM ( '' )  );
#2732 = CARTESIAN_POINT ( 'NONE',  ( -3.756430356249995661, -6.831223922626973533, 2.690624999385480276 ) ) ;
#2733 = CARTESIAN_POINT ( 'NONE',  ( -2.000000000000003997, -27.26874999877097139, 5.535898384862238508 ) ) ;
#2734 =( BOUNDED_CURVE ( )  B_SPLINE_CURVE ( 2, ( #19894, #21493, #13764, #3828, #19645, #15614, #23968, #16000, #40 ),
 .UNSPECIFIED., .F., .F. ) 
 B_SPLINE_CURVE_WITH_KNOTS ( ( 3, 2, 2, 2, 3 ),
 ( 0.4250000000000000444, 0.4333333333333333481, 0.4500000000000000111, 0.4666666666666666741, 0.4750000000000000333 ),
 .UNSPECIFIED. ) 
 CURVE ( )  GEOMETRIC_REPRESENTATION_ITEM ( )  RATIONAL_B_SPLINE_CURVE ( ( 0.9330127018922194093, 0.9330127018922196314, 1.000000000000000000, 0.8660254037844387076, 1.000000000000000000, 0.8660254037844387076, 1.000000000000000000, 0.9330127018922191873, 0.9330127018922194093 ) ) 
 REPRESENTATION_ITEM ( '' )  );
#2735 = CARTESIAN_POINT ( 'NONE',  ( 1.878215178125000939, 29.56562499938548427, 12.25316411605952283 ) ) ;
#2736 = CARTESIAN_POINT ( 'NONE',  ( 16.94404624418269023, 22.60090049367499532, 11.30940107675849404 ) ) ;
#2737 = CARTESIAN_POINT ( 'NONE',  ( 5.335677986744693513, -30.63887302793247258, 1.000000000000000000 ) ) ;
#2738 = AXIS2_PLACEMENT_3D ( 'NONE', #8286, #16268, #12339 ) ;
#2739 = CARTESIAN_POINT ( 'NONE',  ( 3.756430356250003655, 28.29062499938548569, 8.999999999999992895 ) ) ;
#2740 = LINE ( 'NONE', #18826, #12558 ) ;
#2741 = DIRECTION ( 'NONE',  ( 1.000000000000000000, 0.000000000000000000, 0.000000000000000000 ) ) ;
#2742 = CARTESIAN_POINT ( 'NONE',  ( 17.46243120409849325, 18.97818073195047361, 12.99999999999999467 ) ) ;
#2743 = CARTESIAN_POINT ( 'NONE',  ( -2.672651547586948120E-15, -26.94062499938548783, 13.33755215474602984 ) ) ;
#2744 = CARTESIAN_POINT ( 'NONE',  ( -30.78811501957148167, -4.393401135980793626, -2.750000000000000000 ) ) ;
#2745 = CARTESIAN_POINT ( 'NONE',  ( -3.469446951953614189E-15, -30.00000000000000355, 8.999999999999992895 ) ) ;
#2746 = FACE_OUTER_BOUND ( 'NONE', #19654, .T. ) ;
#2747 = CARTESIAN_POINT ( 'NONE',  ( -3.999999999999996447, 27.92500000000000071, 8.999999999999992895 ) ) ;
#2748 = EDGE_LOOP ( 'NONE', ( #1866, #288, #10492, #1406 ) ) ;
#2749 = AXIS2_PLACEMENT_3D ( 'NONE', #4983, #24590, #22506 ) ;
#2750 = CARTESIAN_POINT ( 'NONE',  ( 5.112995299272250684E-15, 27.75624999877097565, 4.999999999999992006 ) ) ;
#2752 = ORIENTED_EDGE ( 'NONE', *, *, #6733, .T. ) ;
#2751 = DIRECTION ( 'NONE',  ( -0.7071067811865487940, -0.7071067811865463515, 0.000000000000000000 ) ) ;
#2753 = VERTEX_POINT ( 'NONE', #21444 ) ;
#2754 = VERTEX_POINT ( 'NONE', #3391 ) ;
#2755 = ORIENTED_EDGE ( 'NONE', *, *, #2599, .F. ) ;
#2756 = EDGE_CURVE ( 'NONE', #14800, #4850, #4597, .T. ) ;
#2757 = ORIENTED_EDGE ( 'NONE', *, *, #13499, .F. ) ;
#2758 = FACE_OUTER_BOUND ( 'NONE', #3165, .T. ) ;
#2759 = VERTEX_POINT ( 'NONE', #19468 ) ;
#2760 = DIRECTION ( 'NONE',  ( 1.000000000000000000, 0.000000000000000000, 0.000000000000000000 ) ) ;
#2761 = CARTESIAN_POINT ( 'NONE',  ( 3.756430356250003655, 27.95312499938548711, 8.999999999999992895 ) ) ;
#2762 = EDGE_CURVE ( 'NONE', #18175, #2002, #17007, .T. ) ;
#2763 = CARTESIAN_POINT ( 'NONE',  ( 1.878215178125000939, -12.25316411605952283, 3.328124999385485783 ) ) ;
#2764 = CARTESIAN_POINT ( 'NONE',  ( -1.952785157361201618, 31.03863125411927371, 1.000000000000000000 ) ) ;
#2765 = CARTESIAN_POINT ( 'NONE',  ( 23.32360276639294128, 18.01120801047411746, 6.831223922626973533 ) ) ;
#2766 = EDGE_CURVE ( 'NONE', #25364, #18910, #3342, .T. ) ;
#2767 = CARTESIAN_POINT ( 'NONE',  ( 17.55392584295608316, 23.21078009244839180, 8.999999999999992895 ) ) ;
#2768 = CARTESIAN_POINT ( 'NONE',  ( -31.03863125411922752, 1.952785157361987878, -6.500000000000000000 ) ) ;
#2769 = CARTESIAN_POINT ( 'NONE',  ( 3.756430356250003655, -8.999999999999992895, 3.290624999385483029 ) ) ;
#2770 = DIRECTION ( 'NONE',  ( -0.000000000000000000, -0.000000000000000000, 1.000000000000000000 ) ) ;
#2772 = EDGE_CURVE ( 'NONE', #2907, #4929, #9413, .T. ) ;
#2771 = CARTESIAN_POINT ( 'NONE',  ( 2.620986760973688460E-15, -13.61880215351699874, 3.487499999999998934 ) ) ;
#2773 = CARTESIAN_POINT ( 'NONE',  ( -1.071796769724483456, 28.67634618820330772, 4.999999999999992006 ) ) ;
#2774 = CARTESIAN_POINT ( 'NONE',  ( 1.878215178125004048, -5.746835883940462963, 3.028124999385484184 ) ) ;
#2775 = LINE ( 'NONE', #12588, #4943 ) ;
#2776 = DIRECTION ( 'NONE',  ( 0.000000000000000000, 1.000000000000000000, -0.000000000000000000 ) ) ;
#2777 = ORIENTED_EDGE ( 'NONE', *, *, #136, .T. ) ;
#2778 = ORIENTED_EDGE ( 'NONE', *, *, #24551, .F. ) ;
#2779 = CARTESIAN_POINT ( 'NONE',  ( 1.878215178125008489, 28.92812499938549209, 5.746835883940462963 ) ) ;
#2780 = EDGE_CURVE ( 'NONE', #20797, #6542, #17, .T. ) ;
#2781 = ORIENTED_EDGE ( 'NONE', *, *, #1250, .T. ) ;
#2782 = CARTESIAN_POINT ( 'NONE',  ( 27.49048467073848911, -14.54246377227368647, 1.000000000000000000 ) ) ;
#2783 = ORIENTED_EDGE ( 'NONE', *, *, #15065, .F. ) ;
#2784 = CARTESIAN_POINT ( 'NONE',  ( 3.756430356249995661, -25.44062499938548427, 6.831223922626973533 ) ) ;
#2785 = ORIENTED_EDGE ( 'NONE', *, *, #3875, .T. ) ;
#2786 = CARTESIAN_POINT ( 'NONE',  ( 3.469446951953614189E-15, -8.999999999999992895, 6.000000000000000000 ) ) ;
#2787 = VERTEX_POINT ( 'NONE', #13479 ) ;
#2788 = CYLINDRICAL_SURFACE ( 'NONE', #25222, 30.10000000000000142 ) ;
#2789 = CARTESIAN_POINT ( 'NONE',  ( -3.756430356249995661, 28.92812499938548143, 6.831223922626973533 ) ) ;
#2790 = CARTESIAN_POINT ( 'NONE',  ( -3.999999999999995559, 28.28124999877096712, 6.690598923241487306 ) ) ;
#2791 = LINE ( 'NONE', #6852, #16768 ) ;
#2792 = CARTESIAN_POINT ( 'NONE',  ( 28.34936733434200207, 12.78762572734058978, 1.000000000000000000 ) ) ;
#2793 = CARTESIAN_POINT ( 'NONE',  ( 15.99595368409253915, 21.30834844001121553, 8.999999999999992895 ) ) ;
#2794 = EDGE_CURVE ( 'NONE', #22706, #23573, #3253, .T. ) ;
#2795 = CARTESIAN_POINT ( 'NONE',  ( 3.756430356250004099, 27.87812499938548427, 6.831223922626973533 ) ) ;
#2796 = EDGE_CURVE ( 'NONE', #21955, #15596, #7439, .T. ) ;
#2797 = DIRECTION ( 'NONE',  ( -0.000000000000000000, 0.000000000000000000, 1.000000000000000000 ) ) ;
#2798 = EDGE_LOOP ( 'NONE', ( #8102, #892, #24766, #13917 ) ) ;
#2799 = CARTESIAN_POINT ( 'NONE',  ( 2.000000000000003997, -5.535898384862238508, 3.168749998770967302 ) ) ;
#2800 = LINE ( 'NONE', #470, #5913 ) ;
#2801 = EDGE_CURVE ( 'NONE', #22370, #19772, #25694, .T. ) ;
#2802 = FACE_OUTER_BOUND ( 'NONE', #6159, .T. ) ;
#2803 = CARTESIAN_POINT ( 'NONE',  ( -3.756430356250002323, -28.25312499938548427, 11.16877607737301403 ) ) ;
#2804 = EDGE_CURVE ( 'NONE', #7472, #12264, #5614, .T. ) ;
#2805 = CARTESIAN_POINT ( 'NONE',  ( 5.297476235640267817, 38.97860908142764913, 10.55769154565112622 ) ) ;
#2806 = CARTESIAN_POINT ( 'NONE',  ( 2.672651547586948120E-15, 25.59062499938548640, 13.33755215474602984 ) ) ;
#2807 = CARTESIAN_POINT ( 'NONE',  ( 3.469446951953614189E-15, -8.999999999999992895, 0.000000000000000000 ) ) ;
#2809 = ORIENTED_EDGE ( 'NONE', *, *, #22800, .F. ) ;
#2808 = CARTESIAN_POINT ( 'NONE',  ( 2.003086131649545506E-15, 29.19062499938548783, 13.33755215474603162 ) ) ;
#2810 = ORIENTED_EDGE ( 'NONE', *, *, #20276, .T. ) ;
#2811 = CARTESIAN_POINT ( 'NONE',  ( -1.859271017917182139E-15, -29.33124999877096428, 12.99999999999999289 ) ) ;
#2812 = EDGE_CURVE ( 'NONE', #16116, #24341, #1256, .T. ) ;
#2813 = CARTESIAN_POINT ( 'NONE',  ( 4.000000000000003553, -8.999999999999992895, 4.443749998770965881 ) ) ;
#2814 = ORIENTED_EDGE ( 'NONE', *, *, #14043, .T. ) ;
#2815 = CARTESIAN_POINT ( 'NONE',  ( -1.878215178125004048, -25.77812499938548640, 5.746835883940462963 ) ) ;
#2816 = DIRECTION ( 'NONE',  ( -0.000000000000000000, 1.000000000000000000, -0.000000000000000000 ) ) ;
#2817 = CARTESIAN_POINT ( 'NONE',  ( -1.878215178124994722, 26.64062499938549067, 5.746835883940462963 ) ) ;
#2818 = CYLINDRICAL_SURFACE ( 'NONE', #154, 0.5000000000000004441 ) ;
#2819 = CARTESIAN_POINT ( 'NONE',  ( 4.000000000000003553, 25.45000000000000639, 8.999999999999992895 ) ) ;
#2820 = CARTESIAN_POINT ( 'NONE',  ( -31.10000000000000142, 3.257552089140643357E-13, -6.500000000000000000 ) ) ;
#2821 = CARTESIAN_POINT ( 'NONE',  ( 2.006336132164985451E-12, 39.00000000001113420, 3.500000000010202061 ) ) ;
#2822 = DIRECTION ( 'NONE',  ( 1.000000000000000000, 0.000000000000000000, 0.000000000000000000 ) ) ;
#2823 = CARTESIAN_POINT ( 'NONE',  ( 3.756430356250003655, 25.25312499938548427, 8.999999999999992895 ) ) ;
#2824 = EDGE_CURVE ( 'NONE', #1894, #20362, #128, .T. ) ;
#2825 = FACE_OUTER_BOUND ( 'NONE', #23704, .T. ) ;
#2826 = AXIS2_PLACEMENT_3D ( 'NONE', #20097, #8083, #10278 ) ;
#2827 = CARTESIAN_POINT ( 'NONE',  ( 17.92073748482754780, 20.74916460957366127, 5.535898384862237620 ) ) ;
#2828 = CARTESIAN_POINT ( 'NONE',  ( -31.10000000000000142, 3.257552089140643357E-13, 1.000000000000000000 ) ) ;
#2829 = CARTESIAN_POINT ( 'NONE',  ( 17.18919637734483885, 22.50159113326351346, 8.999999999999992895 ) ) ;
#2830 = CARTESIAN_POINT ( 'NONE',  ( 16.31415173562648491, 21.62654649154516306, 8.999999999999992895 ) ) ;
#2831 = CARTESIAN_POINT ( 'NONE',  ( -5.840899737312955864, 38.49999999999999289, 10.37254881831481512 ) ) ;
#2832 = DIRECTION ( 'NONE',  ( 0.9048270524660262382, 0.4257792915650585042, 0.000000000000000000 ) ) ;
#2833 = CARTESIAN_POINT ( 'NONE',  ( 3.756430356250003655, 26.94062499938548427, 8.999999999999992895 ) ) ;
#2834 = CARTESIAN_POINT ( 'NONE',  ( -6.317933499823659815, -30.45149776762723093, -6.500000000000000000 ) ) ;
#2835 =( BOUNDED_CURVE ( )  B_SPLINE_CURVE ( 2, ( #14910, #15176, #1047, #18961, #19203, #5345, #23145, #3383, #9282 ),
 .UNSPECIFIED., .F., .F. ) 
 B_SPLINE_CURVE_WITH_KNOTS ( ( 3, 2, 2, 2, 3 ),
 ( 0.6250000000000000000, 0.6333333333333333037, 0.6500000000000000222, 0.6666666666666666297, 0.6750000000000000444 ),
 .UNSPECIFIED. ) 
 CURVE ( )  GEOMETRIC_REPRESENTATION_ITEM ( )  RATIONAL_B_SPLINE_CURVE ( ( 0.9330127018922194093, 0.9330127018922194093, 1.000000000000000000, 0.8660254037844387076, 1.000000000000000000, 0.8660254037844387076, 1.000000000000000000, 0.9330127018922189652, 0.9330127018922194093 ) ) 
 REPRESENTATION_ITEM ( '' )  );
#2836 = CARTESIAN_POINT ( 'NONE',  ( 20.72498534553237093, 15.41259058961355954, 11.16877607737301403 ) ) ;
#2837 = CARTESIAN_POINT ( 'NONE',  ( -18.68225429291695860, 24.86329371854795056, -6.500000000000000000 ) ) ;
#2838 = VERTEX_POINT ( 'NONE', #21562 ) ;
#2839 = CARTESIAN_POINT ( 'NONE',  ( 3.834746474454188013E-15, 27.81249999999999645, 4.999999999999992006 ) ) ;
#2840 = CARTESIAN_POINT ( 'NONE',  ( 2.000000000000000888, 28.46874999877097068, 12.46410161513774817 ) ) ;
#2841 = CARTESIAN_POINT ( 'NONE',  ( -3.756430356250004099, -28.77812499938548285, 6.831223922626973533 ) ) ;
#2843 = ORIENTED_EDGE ( 'NONE', *, *, #22743, .F. ) ;
#2842 = CARTESIAN_POINT ( 'NONE',  ( -14.98253926456356666, -27.25313774936403988, 1.000000000000000000 ) ) ;
#2844 = CARTESIAN_POINT ( 'NONE',  ( 16.66421332384682685, 26.25859848311265310, 1.000000000000000000 ) ) ;
#2845 = ADVANCED_FACE ( 'NONE', ( #17653 ), #23918, .T. ) ;
#2846 = ORIENTED_EDGE ( 'NONE', *, *, #15366, .F. ) ;
#2847 = CARTESIAN_POINT ( 'NONE',  ( -1.878215178125004048, -25.66562499938548569, 5.746835883940462963 ) ) ;
#2848 = VERTEX_POINT ( 'NONE', #11997 ) ;
#2849 = ORIENTED_EDGE ( 'NONE', *, *, #20421, .F. ) ;
#2850 = DIRECTION ( 'NONE',  ( -0.1253332335642912687, 0.9921147013144795412, 0.000000000000000000 ) ) ;
#2851 = CARTESIAN_POINT ( 'NONE',  ( 8.012344526598182026E-15, 28.06562499938548783, 4.662447845253954171 ) ) ;
#2852 = CIRCLE ( 'NONE', #20811, 31.10000000000000142 ) ;
#2853 = CARTESIAN_POINT ( 'NONE',  ( -3.999999999999973355, -6.690598923241474871, 1.987499999999999600 ) ) ;
#2854 = AXIS2_PLACEMENT_3D ( 'NONE', #22092, #6022, #24187 ) ;
#2855 = CARTESIAN_POINT ( 'NONE',  ( 3.735045420075836212E-15, -4.662447845253954171, 2.615624999385482319 ) ) ;
#2856 = CARTESIAN_POINT ( 'NONE',  ( 3.137519842735244810E-15, -27.30624999877096926, 4.999999999999991118 ) ) ;
#2857 = CARTESIAN_POINT ( 'NONE',  ( -3.756430356249995661, 28.47812499938548569, 6.831223922626973533 ) ) ;
#2858 = LINE ( 'NONE', #4711, #11722 ) ;
#2859 = FACE_OUTER_BOUND ( 'NONE', #16413, .T. ) ;
#2860 = UNCERTAINTY_MEASURE_WITH_UNIT (LENGTH_MEASURE( 1.000000000000000082E-05 ), #7555, 'distance_accuracy_value', 'NONE');
#2861 = PRODUCT_DEFINITION_CONTEXT ( 'detailed design', #19293, 'design' ) ;
#2862 = CARTESIAN_POINT ( 'NONE',  ( -1.878215178124995832, 28.44062499938548427, 5.746835883940462963 ) ) ;
#2863 = DIRECTION ( 'NONE',  ( 0.000000000000000000, 0.000000000000000000, 1.000000000000000000 ) ) ;
#2864 = CARTESIAN_POINT ( 'NONE',  ( 4.000000000000003553, 25.84374999877096712, 8.999999999999992895 ) ) ;
#2865 = CARTESIAN_POINT ( 'NONE',  ( -11.44867358849371541, -28.91604871112453168, -6.500000000000000000 ) ) ;
#2866 = CARTESIAN_POINT ( 'NONE',  ( 3.756430356249995661, -26.79062499938548925, 6.831223922626973533 ) ) ;
#2867 = CARTESIAN_POINT ( 'NONE',  ( -1.878215178124995832, 25.85312499938548569, 5.746835883940462963 ) ) ;
#2868 = CIRCLE ( 'NONE', #2026, 0.4999999999999989453 ) ;
#2869 = DIRECTION ( 'NONE',  ( 1.000000000000000000, 0.000000000000000000, 0.000000000000000000 ) ) ;
#2870 = CARTESIAN_POINT ( 'NONE',  ( 1.289143957944685281, -29.97326948525437729, 12.79562863665509553 ) ) ;
#2871 = ADVANCED_FACE ( 'NONE', ( #3642 ), #22070, .T. ) ;
#2873 = ORIENTED_EDGE ( 'NONE', *, *, #20339, .F. ) ;
#2872 = CIRCLE ( 'NONE', #17488, 0.5000000000000000000 ) ;
#2874 = FACE_OUTER_BOUND ( 'NONE', #15489, .T. ) ;
#2876 = VERTEX_POINT ( 'NONE', #13983 ) ;
#2875 = DIRECTION ( 'NONE',  ( 1.000000000000000000, 0.000000000000000000, 0.000000000000000000 ) ) ;
#2877 = AXIS2_PLACEMENT_3D ( 'NONE', #20857, #19281, #23091 ) ;
#2878 = ORIENTED_EDGE ( 'NONE', *, *, #14687, .T. ) ;
#2880 = VERTEX_POINT ( 'NONE', #6122 ) ;
#2879 = VECTOR ( 'NONE', #23809, 1000.000000000000000 ) ;
#2881 = ORIENTED_EDGE ( 'NONE', *, *, #11890, .T. ) ;
#2882 = ORIENTED_EDGE ( 'NONE', *, *, #11177, .F. ) ;
#2883 = CARTESIAN_POINT ( 'NONE',  ( 30.45149776762725224, -6.317933499823547017, -6.500000000000000000 ) ) ;
#2884 = ORIENTED_EDGE ( 'NONE', *, *, #22262, .T. ) ;
#2885 = CARTESIAN_POINT ( 'NONE',  ( 3.469446951953614189E-15, 35.50000000000000711, 8.999999999999992895 ) ) ;
#2886 = CARTESIAN_POINT ( 'NONE',  ( 2.672651547586948120E-15, 29.19062499938548427, 13.33755215474603162 ) ) ;
#2887 =( BOUNDED_CURVE ( )  B_SPLINE_CURVE ( 2, ( #25233, #21300, #21053, #8899, #8753, #5098, #6922 ),
 .UNSPECIFIED., .F., .F. ) 
 B_SPLINE_CURVE_WITH_KNOTS ( ( 3, 2, 2, 3 ),
 ( 0.04999999999999990563, 0.06666666666666654084, 0.08333333333333316217, 0.09999999999999981126 ),
 .UNSPECIFIED. ) 
 CURVE ( )  GEOMETRIC_REPRESENTATION_ITEM ( )  RATIONAL_B_SPLINE_CURVE ( ( 1.000000000000000666, 0.8660254037844378194, 1.000000000000000000, 0.8660254037844387076, 1.000000000000000000, 0.8660254037844402619, 0.9999999999999984457 ) ) 
 REPRESENTATION_ITEM ( '' )  );
#2888 = AXIS2_PLACEMENT_3D ( 'NONE', #5067, #6893, #15144 ) ;
#2889 = CARTESIAN_POINT ( 'NONE',  ( 1.878215178125004048, -5.746835883940462963, 3.928124999385485872 ) ) ;
#2890 = CARTESIAN_POINT ( 'NONE',  ( 4.000000000000001776, 29.46250000000000213, 11.30940107675849760 ) ) ;
#2891 = CARTESIAN_POINT ( 'NONE',  ( 3.735045420075836212E-15, 26.71562499938548640, 4.662447845253954171 ) ) ;
#2892 = CIRCLE ( 'NONE', #10395, 4.000000000000000000 ) ;
#2893 = CARTESIAN_POINT ( 'NONE',  ( 17.18149551509901585, -19.58805710660145749, 20.00001200000000168 ) ) ;
#2894 = VECTOR ( 'NONE', #18580, 1000.000000000000000 ) ;
#2895 = CARTESIAN_POINT ( 'NONE',  ( 4.000000000000001776, -11.30940107675849760, 0.4124999999999987566 ) ) ;
#2896 = ADVANCED_FACE ( 'NONE', ( #3775 ), #25623, .T. ) ;
#2897 = DIRECTION ( 'NONE',  ( 0.000000000000000000, 0.000000000000000000, -1.000000000000000000 ) ) ;
#2898 = CYLINDRICAL_SURFACE ( 'NONE', #16642, 4.000000000000000000 ) ;
#2899 = DIRECTION ( 'NONE',  ( 0.000000000000000000, 0.000000000000000000, 1.000000000000000000 ) ) ;
#2900 = LINE ( 'NONE', #9048, #3802 ) ;
#2901 = CARTESIAN_POINT ( 'NONE',  ( 3.756430356250003211, -6.831223922626973533, 2.090624999385480631 ) ) ;
#2902 = CARTESIAN_POINT ( 'NONE',  ( 1.626862140677534194E-14, 27.98124999877096997, 12.99999999999999289 ) ) ;
#2903 = EDGE_CURVE ( 'NONE', #17608, #5905, #25059, .T. ) ;
#2904 = AXIS2_PLACEMENT_3D ( 'NONE', #9180, #7226, #15209 ) ;
#2905 = DIRECTION ( 'NONE',  ( 0.000000000000000000, 0.000000000000000000, 1.000000000000000000 ) ) ;
#2906 = VERTEX_POINT ( 'NONE', #25874 ) ;
#2907 = VERTEX_POINT ( 'NONE', #21951 ) ;
#2908 = VECTOR ( 'NONE', #7277, 1000.000000000000000 ) ;
#2909 = EDGE_CURVE ( 'NONE', #14282, #4475, #7706, .T. ) ;
#2911 = ORIENTED_EDGE ( 'NONE', *, *, #24526, .F. ) ;
#2910 = AXIS2_PLACEMENT_3D ( 'NONE', #13480, #17897, #25875 ) ;
#2912 = CARTESIAN_POINT ( 'NONE',  ( 0.000000000000000000, 0.000000000000000000, 1.000000000000000000 ) ) ;
#2913 = ORIENTED_EDGE ( 'NONE', *, *, #13233, .T. ) ;
#2914 = CARTESIAN_POINT ( 'NONE',  ( -3.756430356250003655, -26.60312499938548569, 8.999999999999992895 ) ) ;
#2915 = EDGE_CURVE ( 'NONE', #19787, #21069, #1830, .T. ) ;
#2916 = ORIENTED_EDGE ( 'NONE', *, *, #3429, .T. ) ;
#2917 = CARTESIAN_POINT ( 'NONE',  ( 5.112995299272250684E-15, 27.75624999877097565, 4.999999999999992006 ) ) ;
#2918 = AXIS2_PLACEMENT_3D ( 'NONE', #2764, #11001, #17022 ) ;
#2919 = AXIS2_PLACEMENT_3D ( 'NONE', #19547, #8182, #9876 ) ;
#2920 = ORIENTED_EDGE ( 'NONE', *, *, #2122, .F. ) ;
#2921 = APPLICATION_CONTEXT ( 'automotive_design' ) ;
#2922 = EDGE_CURVE ( 'NONE', #2906, #414, #9197, .T. ) ;
#2923 = DIRECTION ( 'NONE',  ( 0.000000000000000000, 0.000000000000000000, 1.000000000000000000 ) ) ;
#2924 = CARTESIAN_POINT ( 'NONE',  ( -1.999999999999998224, 25.75000000000000355, 12.46410161513774639 ) ) ;
#2925 = CARTESIAN_POINT ( 'NONE',  ( 1.071796769724491227, 27.28615380933863577, 4.999999999999989342 ) ) ;
#2926 = VECTOR ( 'NONE', #17138, 1000.000000000000000 ) ;
#2927 = FACE_OUTER_BOUND ( 'NONE', #23153, .T. ) ;
#2928 = CARTESIAN_POINT ( 'NONE',  ( -1.999999999999998224, 28.39374999877096784, 12.46410161513774639 ) ) ;
#2929 = CARTESIAN_POINT ( 'NONE',  ( 22.13036007314063625, 16.81796531722181598, 6.831223922626973533 ) ) ;
#2930 = CIRCLE ( 'NONE', #9201, 31.10000000000000142 ) ;
#2931 = CARTESIAN_POINT ( 'NONE',  ( -1.071796769724488563, 28.46740381056766722, 12.99999999999999289 ) ) ;
#2932 = CARTESIAN_POINT ( 'NONE',  ( 1.878215178125004048, 27.46562499938548640, 5.746835883940462963 ) ) ;
#2933 = CIRCLE ( 'NONE', #15893, 4.000000000000000000 ) ;
#2934 = CARTESIAN_POINT ( 'NONE',  ( 15.67775563255858984, 20.99015038847727155, 8.999999999999992895 ) ) ;
#2935 = CARTESIAN_POINT ( 'NONE',  ( 0.000000000000000000, 31.10000000000000142, 1.000000000000000000 ) ) ;
#2936 = EDGE_LOOP ( 'NONE', ( #14382, #3286, #21484, #21600 ) ) ;
#2937 = FACE_OUTER_BOUND ( 'NONE', #17685, .T. ) ;
#2938 = CARTESIAN_POINT ( 'NONE',  ( -3.999999999999997335, 29.31250000000000000, 11.30940107675849404 ) ) ;
#2939 = CARTESIAN_POINT ( 'NONE',  ( 3.756430356249996105, -26.67812499938548498, 6.831223922626973533 ) ) ;
#2940 = EDGE_CURVE ( 'NONE', #20602, #3531, #10020, .T. ) ;
#2941 = DIRECTION ( 'NONE',  ( 0.8763066800438685799, 0.4817536741017063306, 0.000000000000000000 ) ) ;
#2942 = CARTESIAN_POINT ( 'NONE',  ( -1.999999999999998224, 29.29374999877096997, 12.46410161513774639 ) ) ;
#2943 = DIRECTION ( 'NONE',  ( 0.000000000000000000, 0.000000000000000000, -1.000000000000000000 ) ) ;
#2945 = ORIENTED_EDGE ( 'NONE', *, *, #12834, .T. ) ;
#2944 = CARTESIAN_POINT ( 'NONE',  ( 3.756430356250004099, 28.81562499938548783, 11.16877607737301403 ) ) ;
#2946 = ORIENTED_EDGE ( 'NONE', *, *, #3698, .T. ) ;
#2947 = CYLINDRICAL_SURFACE ( 'NONE', #25419, 0.5000000000000004441 ) ;
#2948 = CIRCLE ( 'NONE', #13807, 0.5000000000000003331 ) ;
#2949 = CIRCLE ( 'NONE', #6693, 0.5000000000000004441 ) ;
#2950 = CARTESIAN_POINT ( 'NONE',  ( 4.000000000000002665, 27.28749999999999787, 6.690598923241489970 ) ) ;
#2951 = ORIENTED_EDGE ( 'NONE', *, *, #17946, .T. ) ;
#2952 = EDGE_CURVE ( 'NONE', #21505, #13603, #3912, .T. ) ;
#2953 = AXIS2_PLACEMENT_3D ( 'NONE', #18009, #8314, #18527 ) ;
#2954 = CARTESIAN_POINT ( 'NONE',  ( -1.878215178125004048, -28.92812499938548854, 5.746835883940462963 ) ) ;
#2955 = CARTESIAN_POINT ( 'NONE',  ( 1.071796769724492338, 25.80759618943233491, 12.99999999999999467 ) ) ;
#2956 = CARTESIAN_POINT ( 'NONE',  ( 3.756430356250004099, 26.07812499938549067, 6.831223922626973533 ) ) ;
#2958 = ADVANCED_FACE ( 'NONE', ( #25742 ), #21757, .F. ) ;
#2957 = AXIS2_PLACEMENT_3D ( 'NONE', #24182, #8117, #20255 ) ;
#2959 = LINE ( 'NONE', #621, #13533 ) ;
#2960 = CARTESIAN_POINT ( 'NONE',  ( 1.878215178125006934, 29.26562499938549067, 5.746835883940462963 ) ) ;
#2961 = AXIS2_PLACEMENT_3D ( 'NONE', #23328, #5419, #13403 ) ;
#2962 = LINE ( 'NONE', #1003, #6270 ) ;
#2963 = DIRECTION ( 'NONE',  ( 1.000000000000000000, 0.000000000000000000, 0.000000000000000000 ) ) ;
#2964 = VECTOR ( 'NONE', #10548, 1000.000000000000000 ) ;
#2965 = CARTESIAN_POINT ( 'NONE',  ( 14.98253926456337837, 27.25313774936414291, -6.500000000000000000 ) ) ;
#2966 = CYLINDRICAL_SURFACE ( 'NONE', #13424, 31.10000000000000142 ) ;
#2967 = CARTESIAN_POINT ( 'NONE',  ( 1.071796769724494558, 25.54240381056766651, 4.999999999999992895 ) ) ;
#2968 = CARTESIAN_POINT ( 'NONE',  ( 23.61528431363239022, 18.30288955771356640, 8.999999999999992895 ) ) ;
#2969 = CARTESIAN_POINT ( 'NONE',  ( 21.78564551731219723, 16.47325076139337696, 8.999999999999992895 ) ) ;
#2970 = CARTESIAN_POINT ( 'NONE',  ( -1.071796769724487230, 28.28259618943233988, 4.999999999999992006 ) ) ;
#2971 = DIRECTION ( 'NONE',  ( 0.000000000000000000, 0.000000000000000000, 1.000000000000000000 ) ) ;
#2972 = CARTESIAN_POINT ( 'NONE',  ( 3.756430356250002323, 28.70312499938548356, 11.16877607737301226 ) ) ;
#2973 = DIRECTION ( 'NONE',  ( 0.000000000000000000, 0.000000000000000000, 1.000000000000000000 ) ) ;
#2974 = CARTESIAN_POINT ( 'NONE',  ( 19.92494326818769323, 19.92494326818762218, 13.33755215474603162 ) ) ;
#2975 = CARTESIAN_POINT ( 'NONE',  ( 29.72853858738278987, -9.133673601486577809, 1.000000000000000000 ) ) ;
#2976 = ORIENTED_EDGE ( 'NONE', *, *, #24436, .T. ) ;
#2977 = CARTESIAN_POINT ( 'NONE',  ( 0.000000000000000000, 0.000000000000000000, 1.000000000000000000 ) ) ;
#2978 = CARTESIAN_POINT ( 'NONE',  ( 2.620986760973688460E-15, 27.08124999877096784, 13.61880215351699874 ) ) ;
#2979 = CARTESIAN_POINT ( 'NONE',  ( -1.878215178125004048, -28.81562499938548427, 5.746835883940462963 ) ) ;
#2981 = EDGE_LOOP ( 'NONE', ( #7500, #17396, #15813, #10815 ) ) ;
#2980 = CARTESIAN_POINT ( 'NONE',  ( -1.071796769724487230, 25.52634618820330559, 4.999999999999992006 ) ) ;
#2982 = DIRECTION ( 'NONE',  ( 0.000000000000000000, 0.000000000000000000, -1.000000000000000000 ) ) ;
#2983 = AXIS2_PLACEMENT_3D ( 'NONE', #9865, #5809, #2020 ) ;
#2984 = EDGE_LOOP ( 'NONE', ( #16925, #4086, #24094, #23586 ) ) ;
#2985 = EDGE_CURVE ( 'NONE', #256, #20149, #3675, .T. ) ;
#2986 = CARTESIAN_POINT ( 'NONE',  ( 3.756430356249996994, -28.51562499938548356, 8.999999999999992895 ) ) ;
#2987 = EDGE_LOOP ( 'NONE', ( #21157, #16477, #16651, #17394 ) ) ;
#2988 = ORIENTED_EDGE ( 'NONE', *, *, #21118, .F. ) ;
#2989 = CARTESIAN_POINT ( 'NONE',  ( 3.469446951953614189E-15, 31.50000000000000000, 8.999999999999992895 ) ) ;
#2990 = AXIS2_PLACEMENT_3D ( 'NONE', #6251, #22211, #18285 ) ;
#2991 = CARTESIAN_POINT ( 'NONE',  ( -1.878215178124999829, 27.80312499938548854, 12.25316411605951927 ) ) ;
#2992 = EDGE_CURVE ( 'NONE', #9030, #7533, #16678, .T. ) ;
#2993 = DIRECTION ( 'NONE',  ( 1.000000000000000000, 0.000000000000000000, 0.000000000000000000 ) ) ;
#2994 = VECTOR ( 'NONE', #13283, 1000.000000000000000 ) ;
#2995 = CARTESIAN_POINT ( 'NONE',  ( 3.756430356250003655, -8.999999999999992895, 2.503124999385482941 ) ) ;
#2996 =( NAMED_UNIT ( * ) SI_UNIT ( $, .STERADIAN. ) SOLID_ANGLE_UNIT ( ) );
#2997 = CARTESIAN_POINT ( 'NONE',  ( -3.526711513758413297, 38.89679573513893729, 4.645898033752330569 ) ) ;
#2998 = CARTESIAN_POINT ( 'NONE',  ( 3.756430356250004099, 27.42812499938548143, 6.831223922626973533 ) ) ;
#2999 = AXIS2_PLACEMENT_3D ( 'NONE', #9884, #3615, #11585 ) ;
#3000 = CYLINDRICAL_SURFACE ( 'NONE', #19238, 31.10000000000000142 ) ;
#3001 = CARTESIAN_POINT ( 'NONE',  ( -3.756430356249996105, 28.47812499938548569, 6.831223922626973533 ) ) ;
#3002 = CYLINDRICAL_SURFACE ( 'NONE', #20478, 0.5000000000000000000 ) ;
#3003 = DIRECTION ( 'NONE',  ( -1.000000000000000000, 0.000000000000000000, 0.000000000000000000 ) ) ;
#3004 = CARTESIAN_POINT ( 'NONE',  ( -4.393401135981330086, -30.78811501957140351, -6.500000000000000000 ) ) ;
#3005 = CARTESIAN_POINT ( 'NONE',  ( 30.63887302793244061, -5.335677986744896906, 1.000000000000000000 ) ) ;
#3006 = CARTESIAN_POINT ( 'NONE',  ( 3.756430356249997882, -27.31562499938548427, 11.16877607737301226 ) ) ;
#3007 = AXIS2_PLACEMENT_3D ( 'NONE', #5748, #13734, #21711 ) ;
#3008 = CARTESIAN_POINT ( 'NONE',  ( 3.735045420075836212E-15, 26.26562499938548356, 4.662447845253954171 ) ) ;
#3009 = CIRCLE ( 'NONE', #7174, 0.4999999999999991673 ) ;
#3010 = CARTESIAN_POINT ( 'NONE',  ( -1.071796769724493448, 29.57634618820329564, 4.999999999999995559 ) ) ;
#3011 = CARTESIAN_POINT ( 'NONE',  ( -3.369928719974892281E-15, -25.11250000000000426, 4.999999999999992006 ) ) ;
#3012 = LINE ( 'NONE', #19083, #140 ) ;
#3013 = ORIENTED_EDGE ( 'NONE', *, *, #24748, .F. ) ;
#3014 = DIRECTION ( 'NONE',  ( -0.000000000000000000, 0.000000000000000000, -1.000000000000000000 ) ) ;
#3016 = ORIENTED_EDGE ( 'NONE', *, *, #24073, .F. ) ;
#3015 = CYLINDRICAL_SURFACE ( 'NONE', #4153, 31.10000000000000142 ) ;
#3017 = AXIS2_PLACEMENT_3D ( 'NONE', #21054, #1045, #303 ) ;
#3018 = VERTEX_POINT ( 'NONE', #12234 ) ;
#3019 = ORIENTED_EDGE ( 'NONE', *, *, #5268, .T. ) ;
#3020 = EDGE_LOOP ( 'NONE', ( #7483, #3106, #5006, #12106 ) ) ;
#3021 = ORIENTED_EDGE ( 'NONE', *, *, #17150, .F. ) ;
#3022 = EDGE_CURVE ( 'NONE', #11790, #1277, #20201, .T. ) ;
#3023 = FACE_OUTER_BOUND ( 'NONE', #12961, .T. ) ;
#3024 = AXIS2_PLACEMENT_3D ( 'NONE', #18051, #19979, #4166 ) ;
#3025 = VERTEX_POINT ( 'NONE', #18252 ) ;
#3026 = PLANE ( 'NONE',  #8587 ) ;
#3027 = CARTESIAN_POINT ( 'NONE',  ( -1.878215178124998497, 27.80312499938548498, 12.25316411605951927 ) ) ;
#3028 = AXIS2_PLACEMENT_3D ( 'NONE', #13833, #18269, #24141 ) ;
#3029 = EDGE_CURVE ( 'NONE', #15016, #11472, #8357, .T. ) ;
#3030 = CIRCLE ( 'NONE', #5124, 31.10000000000000142 ) ;
#3031 = CARTESIAN_POINT ( 'NONE',  ( -3.756430356249996994, -8.999999999999992895, 0.8156249993854814972 ) ) ;
#3032 = DIRECTION ( 'NONE',  ( 1.000000000000000000, 0.000000000000000000, 0.000000000000000000 ) ) ;
#3033 = CARTESIAN_POINT ( 'NONE',  ( 22.63417365473605614, 17.32177889881723587, 11.16877607737301226 ) ) ;
#3034 = CARTESIAN_POINT ( 'NONE',  ( 3.735045420075836212E-15, 25.81562499938548783, 4.662447845253954171 ) ) ;
#3035 = EDGE_CURVE ( 'NONE', #24788, #6934, #13017, .T. ) ;
#3036 = CARTESIAN_POINT ( 'NONE',  ( -26.00000000000000355, -1.701696020694477784, 20.00001200000000523 ) ) ;
#3037 = CARTESIAN_POINT ( 'NONE',  ( 3.756430356250003655, -8.999999999999992895, 3.740624999385481875 ) ) ;
#3038 = DIRECTION ( 'NONE',  ( -1.000000000000000000, 0.000000000000000000, 0.000000000000000000 ) ) ;
#3039 = CARTESIAN_POINT ( 'NONE',  ( 4.000000000000003553, -6.690598923241489970, 3.187499999999998668 ) ) ;
#3040 = DIRECTION ( 'NONE',  ( -0.8763066800438602533, 0.4817536741017213187, 0.000000000000000000 ) ) ;
#3041 = CARTESIAN_POINT ( 'NONE',  ( 2.672651547586948120E-15, -13.33755215474603162, 3.290624999385483918 ) ) ;
#3042 = CARTESIAN_POINT ( 'NONE',  ( 0.000000000000000000, 0.000000000000000000, 1.000000000000000000 ) ) ;
#3043 = VECTOR ( 'NONE', #4699, 1000.000000000000000 ) ;
#3044 = CARTESIAN_POINT ( 'NONE',  ( -4.000000000000003553, -25.44999999999999929, 8.999999999999992895 ) ) ;
#3045 = ORIENTED_EDGE ( 'NONE', *, *, #13540, .F. ) ;
#3046 = ORIENTED_EDGE ( 'NONE', *, *, #23099, .F. ) ;
#3047 = CIRCLE ( 'NONE', #9302, 0.7500000000000001110 ) ;
#3048 = ORIENTED_EDGE ( 'NONE', *, *, #8670, .F. ) ;
#3049 = CARTESIAN_POINT ( 'NONE',  ( -18.68225429291695860, 24.86329371854795056, 1.000000000000000000 ) ) ;
#3050 = ORIENTED_EDGE ( 'NONE', *, *, #16961, .F. ) ;
#3051 = CARTESIAN_POINT ( 'NONE',  ( -3.756430356250004099, -25.29062499938548569, 6.831223922626973533 ) ) ;
#3052 = EDGE_LOOP ( 'NONE', ( #13152, #12062 ) ) ;
#3053 =( BOUNDED_SURFACE ( )  B_SPLINE_SURFACE ( 1, 2, ( 
 ( #23602, #19669, #5561, #21389, #3589, #13275, #1630, #3469, #11441, #15754, #11307, #23717, #3329, #19413, #1506, #9477, #17455, #25425, #7512, #15506, #23473, #17590, #23987, #4487, #2017, #17978, #11946, #14181, #9985, #19916, #68, #24383, #18503, #18235, #3981, #22407, #16023, #16273, #2155, #12076, #20307, #6460, #24242, #12463, #10358, #12215, #10123, #16539, #20436, #14447, #8041, #2401, #16415, #5944, #12343, #195, #10238, #457, #2534, #10503, #18359, #8428, #4098, #6330, #591, #6070, #8557, #13930, #6191, #22151, #21898, #14053, #18122, #22019, #8168, #20050, #16147, #24108, #4236, #20184, #2283, #318, #8289, #14323, #22287, #4366, #25016, #3057, #10884, #8953, #708, #16927, #1214, #9195, #7105, #14705, #8676, #13129, #19006, #24895, #22806, #2789, #24501, #16657, #971, #14562, #832, #11026, #5153, #6850, #6973, #24624, #10753, #5015, #18884, #6580, #19122, #22543, #4623, #22928, #14953 ),
 ( #1089, #18743, #4883, #18623, #9063, #12606, #17045, #15090, #12856, #10631, #2671, #12997, #20833, #20581, #6710, #23068, #20977, #8809, #16802, #21099, #2924, #22683, #4768, #3177, #11143, #12739, #20710, #24768, #14833, #21605, #11801, #17561, #25536, #7621, #21357, #19776, #15607, #1603, #11660, #23576, #11413, #5773, #11271, #9573, #17697, #19637, #13757, #13518, #1872, #21487, #7361, #19256, #21736, #3562, #3820, #11536, #9715, #19503, #5654, #25157, #5270, #13636, #17431, #17183, #7240, #15219, #23692, #23185, #13248, #3682, #1743, #25666, #7745, #25397, #5391, #13382, #21217, #15728, #3298, #1356, #9333, #17317, #19387, #25280, #15339, #23307, #3441, #1480, #9451, #7484, #15473, #23442, #5532, #23961, #7866, #11919, #20155, #21871, #22375, #9834, #4203, #9955, #10331, #17817, #5911, #2255, #19889, #14149, #24348, #18088, #16117, #13899, #8008, #10087, #25782, #18209, #22115, #291, #8260, #6043, #12181 ) ),
 .UNSPECIFIED., .F., .F., .F. ) 
 B_SPLINE_SURFACE_WITH_KNOTS ( ( 2, 2 ),
 ( 3, 2, 2, 2, 2, 2, 2, 2, 2, 2, 2, 2, 2, 2, 2, 2, 2, 2, 2, 2, 2, 2, 2, 2, 2, 2, 2, 2, 2, 2, 2, 2, 2, 2, 2, 2, 2, 2, 2, 2, 2, 2, 2, 2, 2, 2, 2, 2, 2, 2, 2, 2, 2, 2, 2, 2, 2, 2, 2, 2, 3 ),
 ( 0.000000000000000000, 1.000000000000000000 ),
 ( 0.000000000000000000, 0.01666666666666666644, 0.03333333333333333287, 0.05000000000000000278, 0.06666666666666666574, 0.08333333333333332871, 0.1000000000000000056, 0.1166666666666666685, 0.1333333333333333315, 0.1499999999999999944, 0.1666666666666666574, 0.1833333333333333204, 0.2000000000000000111, 0.2166666666666666741, 0.2333333333333333370, 0.2500000000000000000, 0.2666666666666666630, 0.2833333333333333259, 0.2999999999999999889, 0.3166666666666666519, 0.3333333333333333148, 0.3499999999999999778, 0.3666666666666666408, 0.3833333333333333592, 0.4000000000000000222, 0.4166666666666666852, 0.4333333333333333481, 0.4500000000000000111, 0.4666666666666666741, 0.4833333333333333370, 0.5000000000000000000, 0.5166666666666667185, 0.5333333333333333259, 0.5500000000000000444, 0.5666666666666666519, 0.5833333333333333703, 0.5999999999999999778, 0.6166666666666666963, 0.6333333333333333037, 0.6500000000000000222, 0.6666666666666666297, 0.6833333333333333481, 0.6999999999999999556, 0.7166666666666666741, 0.7333333333333332815, 0.7500000000000000000, 0.7666666666666667185, 0.7833333333333333259, 0.8000000000000000444, 0.8166666666666666519, 0.8333333333333333703, 0.8499999999999999778, 0.8666666666666666963, 0.8833333333333333037, 0.9000000000000000222, 0.9166666666666666297, 0.9333333333333333481, 0.9499999999999999556, 0.9666666666666666741, 0.9833333333333332815, 1.000000000000000000 ),
 .UNSPECIFIED. ) 
 GEOMETRIC_REPRESENTATION_ITEM ( )  RATIONAL_B_SPLINE_SURFACE ( (
 ( 1.000000000000000000, 0.8660254037844387076, 1.000000000000000000, 0.8660254037844387076, 1.000000000000000000, 0.8660254037844387076, 1.000000000000000000, 0.8660254037844387076, 1.000000000000000000, 0.8660254037844387076, 1.000000000000000000, 0.8660254037844387076, 1.000000000000000000, 0.8660254037844387076, 1.000000000000000000, 0.8660254037844387076, 1.000000000000000000, 0.8660254037844387076, 1.000000000000000000, 0.8660254037844387076, 1.000000000000000000, 0.8660254037844387076, 1.000000000000000000, 0.8660254037844387076, 1.000000000000000000, 0.8660254037844387076, 1.000000000000000000, 0.8660254037844387076, 1.000000000000000000, 0.8660254037844387076, 1.000000000000000000, 0.8660254037844387076, 1.000000000000000000, 0.8660254037844387076, 1.000000000000000000, 0.8660254037844387076, 1.000000000000000000, 0.8660254037844387076, 1.000000000000000000, 0.8660254037844387076, 1.000000000000000000, 0.8660254037844387076, 1.000000000000000000, 0.8660254037844387076, 1.000000000000000000, 0.8660254037844387076, 1.000000000000000000, 0.8660254037844387076, 1.000000000000000000, 0.8660254037844387076, 1.000000000000000000, 0.8660254037844387076, 1.000000000000000000, 0.8660254037844387076, 1.000000000000000000, 0.8660254037844387076, 1.000000000000000000, 0.8660254037844387076, 1.000000000000000000, 0.8660254037844387076, 1.000000000000000000, 0.8660254037844387076, 1.000000000000000000, 0.8660254037844387076, 1.000000000000000000, 0.8660254037844387076, 1.000000000000000000, 0.8660254037844387076, 1.000000000000000000, 0.8660254037844387076, 1.000000000000000000, 0.8660254037844387076, 1.000000000000000000, 0.8660254037844387076, 1.000000000000000000, 0.8660254037844387076, 1.000000000000000000, 0.8660254037844387076, 1.000000000000000000, 0.8660254037844387076, 1.000000000000000000, 0.8660254037844387076, 1.000000000000000000, 0.8660254037844387076, 1.000000000000000000, 0.8660254037844387076, 1.000000000000000000, 0.8660254037844387076, 1.000000000000000000, 0.8660254037844387076, 1.000000000000000000, 0.8660254037844387076, 1.000000000000000000, 0.8660254037844387076, 1.000000000000000000, 0.8660254037844387076, 1.000000000000000000, 0.8660254037844387076, 1.000000000000000000, 0.8660254037844387076, 1.000000000000000000, 0.8660254037844387076, 1.000000000000000000, 0.8660254037844387076, 1.000000000000000000, 0.8660254037844387076, 1.000000000000000000, 0.8660254037844387076, 1.000000000000000000, 0.8660254037844387076, 1.000000000000000000, 0.8660254037844387076, 1.000000000000000000, 0.8660254037844387076, 1.000000000000000000, 0.8660254037844387076, 1.000000000000000000, 0.8660254037844387076, 1.000000000000000000, 0.8660254037844387076, 1.000000000000000000),
 ( 1.000000000000000000, 0.8660254037844387076, 1.000000000000000000, 0.8660254037844387076, 1.000000000000000000, 0.8660254037844387076, 1.000000000000000000, 0.8660254037844387076, 1.000000000000000000, 0.8660254037844387076, 1.000000000000000000, 0.8660254037844387076, 1.000000000000000000, 0.8660254037844387076, 1.000000000000000000, 0.8660254037844387076, 1.000000000000000000, 0.8660254037844387076, 1.000000000000000000, 0.8660254037844387076, 1.000000000000000000, 0.8660254037844387076, 1.000000000000000000, 0.8660254037844387076, 1.000000000000000000, 0.8660254037844387076, 1.000000000000000000, 0.8660254037844387076, 1.000000000000000000, 0.8660254037844387076, 1.000000000000000000, 0.8660254037844387076, 1.000000000000000000, 0.8660254037844387076, 1.000000000000000000, 0.8660254037844387076, 1.000000000000000000, 0.8660254037844387076, 1.000000000000000000, 0.8660254037844387076, 1.000000000000000000, 0.8660254037844387076, 1.000000000000000000, 0.8660254037844387076, 1.000000000000000000, 0.8660254037844387076, 1.000000000000000000, 0.8660254037844387076, 1.000000000000000000, 0.8660254037844387076, 1.000000000000000000, 0.8660254037844387076, 1.000000000000000000, 0.8660254037844387076, 1.000000000000000000, 0.8660254037844387076, 1.000000000000000000, 0.8660254037844387076, 1.000000000000000000, 0.8660254037844387076, 1.000000000000000000, 0.8660254037844387076, 1.000000000000000000, 0.8660254037844387076, 1.000000000000000000, 0.8660254037844387076, 1.000000000000000000, 0.8660254037844387076, 1.000000000000000000, 0.8660254037844387076, 1.000000000000000000, 0.8660254037844387076, 1.000000000000000000, 0.8660254037844387076, 1.000000000000000000, 0.8660254037844387076, 1.000000000000000000, 0.8660254037844387076, 1.000000000000000000, 0.8660254037844387076, 1.000000000000000000, 0.8660254037844387076, 1.000000000000000000, 0.8660254037844387076, 1.000000000000000000, 0.8660254037844387076, 1.000000000000000000, 0.8660254037844387076, 1.000000000000000000, 0.8660254037844387076, 1.000000000000000000, 0.8660254037844387076, 1.000000000000000000, 0.8660254037844387076, 1.000000000000000000, 0.8660254037844387076, 1.000000000000000000, 0.8660254037844387076, 1.000000000000000000, 0.8660254037844387076, 1.000000000000000000, 0.8660254037844387076, 1.000000000000000000, 0.8660254037844387076, 1.000000000000000000, 0.8660254037844387076, 1.000000000000000000, 0.8660254037844387076, 1.000000000000000000, 0.8660254037844387076, 1.000000000000000000, 0.8660254037844387076, 1.000000000000000000, 0.8660254037844387076, 1.000000000000000000, 0.8660254037844387076, 1.000000000000000000, 0.8660254037844387076, 1.000000000000000000, 0.8660254037844387076, 1.000000000000000000) ) ) 
 REPRESENTATION_ITEM ( '' )  SURFACE ( )  );
#3054 = CIRCLE ( 'NONE', #12225, 0.4999999999999999445 ) ;
#3055 = ORIENTED_EDGE ( 'NONE', *, *, #22866, .T. ) ;
#3056 = CARTESIAN_POINT ( 'NONE',  ( -3.999999999999996447, -8.999999999999992895, 2.474999999999997868 ) ) ;
#3057 = CARTESIAN_POINT ( 'NONE',  ( 3.735045420075836212E-15, 28.40312499938548640, 4.662447845253954171 ) ) ;
#3058 = EDGE_CURVE ( 'NONE', #23094, #22605, #25178, .T. ) ;
#3059 = CARTESIAN_POINT ( 'NONE',  ( 1.859271017917182139E-15, 26.68750000000000000, 12.99999999999999289 ) ) ;
#3060 = CYLINDRICAL_SURFACE ( 'NONE', #17949, 4.000000000000000000 ) ;
#3061 = CARTESIAN_POINT ( 'NONE',  ( 16.95282131294928263, 19.60901869090858796, 5.746835883940462963 ) ) ;
#3062 = DIRECTION ( 'NONE',  ( 1.000000000000000000, 0.000000000000000000, 0.000000000000000000 ) ) ;
#3063 = EDGE_CURVE ( 'NONE', #2607, #4728, #20997, .T. ) ;
#3064 = EDGE_CURVE ( 'NONE', #23924, #18764, #11689, .T. ) ;
#3065 = CARTESIAN_POINT ( 'NONE',  ( -3.999999999999996003, 25.18750000000000000, 6.690598923241487306 ) ) ;
#3066 = CARTESIAN_POINT ( 'NONE',  ( 21.78564551731219723, 16.47325076139337696, 8.999999999999992895 ) ) ;
#3067 = LINE ( 'NONE', #17197, #6170 ) ;
#3068 = ORIENTED_EDGE ( 'NONE', *, *, #25224, .T. ) ;
#3069 = EDGE_CURVE ( 'NONE', #5761, #9189, #3193, .T. ) ;
#3070 = CARTESIAN_POINT ( 'NONE',  ( -1.999999999999998224, 28.39374999877097139, 12.46410161513774639 ) ) ;
#3071 = CARTESIAN_POINT ( 'NONE',  ( -2.672651547586948120E-15, -26.37812499938548427, 13.33755215474603162 ) ) ;
#3072=STYLED_ITEM('',(#25900),#5435);
#3073 = CARTESIAN_POINT ( 'NONE',  ( -1.071796769724490117, 26.93259618943234202, 4.999999999999992895 ) ) ;
#3074 = CARTESIAN_POINT ( 'NONE',  ( 3.756430356250004099, 28.44062499938548783, 6.831223922626973533 ) ) ;
#3075 = DIRECTION ( 'NONE',  ( -0.000000000000000000, 0.000000000000000000, 1.000000000000000000 ) ) ;
#3077 = VERTEX_POINT ( 'NONE', #13150 ) ;
#3076 = CARTESIAN_POINT ( 'NONE',  ( -3.756430356249994329, 29.11562499938548854, 11.16877607737301048 ) ) ;
#3078 = ORIENTED_EDGE ( 'NONE', *, *, #4498, .F. ) ;
#3079 = DIRECTION ( 'NONE',  ( 0.000000000000000000, 0.000000000000000000, 1.000000000000000000 ) ) ;
#3080 = FACE_OUTER_BOUND ( 'NONE', #12480, .T. ) ;
#3081 = ORIENTED_EDGE ( 'NONE', *, *, #13459, .F. ) ;
#3082 = EDGE_CURVE ( 'NONE', #25535, #3881, #18056, .T. ) ;
#3083 = CARTESIAN_POINT ( 'NONE',  ( 1.878215178124998497, -29.15312499938548640, 12.25316411605951927 ) ) ;
#3084 = CARTESIAN_POINT ( 'NONE',  ( -26.52310962334755473, -16.23990935651699985, 1.000000000000000000 ) ) ;
#3085 = CARTESIAN_POINT ( 'NONE',  ( 7.248980000274197977, 30.24338421796781518, -6.500000000000000000 ) ) ;
#3086 = PRESENTATION_LAYER_ASSIGNMENT (  '', '', ( #22295 ) ) ;
#3087 = CARTESIAN_POINT ( 'NONE',  ( -3.834746474454188013E-15, -26.40624999877096357, 4.999999999999992006 ) ) ;
#3088 = CARTESIAN_POINT ( 'NONE',  ( 4.006172263299091013E-15, 28.40312499938548996, 4.662447845253954171 ) ) ;
#3089 = EDGE_CURVE ( 'NONE', #25106, #25535, #15412, .T. ) ;
#3090 = CARTESIAN_POINT ( 'NONE',  ( 1.071796769724494558, 25.35759618943234628, 12.99999999999999467 ) ) ;
#3091 = PRODUCT_CONTEXT ( 'NONE', #25153, 'mechanical' ) ;
#3092 = EDGE_CURVE ( 'NONE', #22272, #24945, #987, .T. ) ;
#3093 = DIRECTION ( 'NONE',  ( 0.000000000000000000, 0.000000000000000000, -1.000000000000000000 ) ) ;
#3094 = DIRECTION ( 'NONE',  ( 0.000000000000000000, 1.000000000000000000, 0.000000000000000000 ) ) ;
#3095 = CARTESIAN_POINT ( 'NONE',  ( 1.878215178125000939, 26.41562499938548214, 12.25316411605952283 ) ) ;
#3096 = DIRECTION ( 'NONE',  ( -0.000000000000000000, 0.000000000000000000, -1.000000000000000000 ) ) ;
#3097 = CARTESIAN_POINT ( 'NONE',  ( 16.68772003600256326, 19.51614716074868028, 5.535898384862237620 ) ) ;
#3098 = CARTESIAN_POINT ( 'NONE',  ( 21.46744746577824969, 16.15505270985943298, 8.999999999999992895 ) ) ;
#3099 = ADVANCED_FACE ( 'NONE', ( #25038, #19143 ), #9217, .F. ) ;
#3100 = DIRECTION ( 'NONE',  ( 0.000000000000000000, 0.000000000000000000, 1.000000000000000000 ) ) ;
#3101 = CARTESIAN_POINT ( 'NONE',  ( -1.878215178124995832, 26.64062499938548711, 5.746835883940462963 ) ) ;
#3102 = ADVANCED_FACE ( 'NONE', ( #7126 ), #10771, .F. ) ;
#3103 = CARTESIAN_POINT ( 'NONE',  ( -29.57785765677917311, 9.610428525061202265, -6.500000000000000000 ) ) ;
#3104 = CARTESIAN_POINT ( 'NONE',  ( 16.55280027427694378, 21.86519503019561839, 8.999999999999992895 ) ) ;
#3105 = DIRECTION ( 'NONE',  ( 0.000000000000000000, 0.000000000000000000, 1.000000000000000000 ) ) ;
#3106 = ORIENTED_EDGE ( 'NONE', *, *, #10429, .T. ) ;
#3107 = CARTESIAN_POINT ( 'NONE',  ( -1.071796769724493448, 28.73259618943232852, 4.999999999999995559 ) ) ;
#3108 = CARTESIAN_POINT ( 'NONE',  ( -3.999999999999996447, 28.31874999877096855, 8.999999999999992895 ) ) ;
#3109 = CARTESIAN_POINT ( 'NONE',  ( 1.878215178124998497, -29.04062499938548569, 12.25316411605951927 ) ) ;
#3111 = EDGE_LOOP ( 'NONE', ( #11503, #18488, #17315, #16475 ) ) ;
#3110 = DIRECTION ( 'NONE',  ( 0.000000000000000000, -0.000000000000000000, 1.000000000000000000 ) ) ;
#3112 = LINE ( 'NONE', #7411, #5393 ) ;
#3113 = ORIENTED_EDGE ( 'NONE', *, *, #1697, .T. ) ;
#3114 = CARTESIAN_POINT ( 'NONE',  ( -1.878215178125004048, -29.26562499938548356, 5.746835883940462963 ) ) ;
#3115 = EDGE_LOOP ( 'NONE', ( #11167, #14069, #8642, #18079 ) ) ;
#3116 = ORIENTED_EDGE ( 'NONE', *, *, #19511, .F. ) ;
#3117 = CARTESIAN_POINT ( 'NONE',  ( 18.21587718922017984, 23.83662110555050617, 8.477544402765669673 ) ) ;
#3118 = CARTESIAN_POINT ( 'NONE',  ( -1.878215178124999829, 26.90312499938548640, 12.25316411605951927 ) ) ;
#3119 = DIRECTION ( 'NONE',  ( 0.000000000000000000, -0.000000000000000000, 1.000000000000000000 ) ) ;
#3120 = CYLINDRICAL_SURFACE ( 'NONE', #20869, 31.10000000000000142 ) ;
#3121 = SURFACE_SIDE_STYLE ('',( #22749 ) ) ;
#3122 = DIRECTION ( 'NONE',  ( 1.000000000000000000, 0.000000000000000000, 0.000000000000000000 ) ) ;
#3123 = CARTESIAN_POINT ( 'NONE',  ( 3.756430356250003655, 29.19062499938548072, 8.999999999999992895 ) ) ;
#3124 = CARTESIAN_POINT ( 'NONE',  ( 4.000000000000005329, 26.80000000000000426, 8.999999999999992895 ) ) ;
#3125 = DIRECTION ( 'NONE',  ( 1.000000000000000000, 0.000000000000000000, 0.000000000000000000 ) ) ;
#3126 = UNCERTAINTY_MEASURE_WITH_UNIT (LENGTH_MEASURE( 1.000000000000000082E-05 ), #6522, 'distance_accuracy_value', 'NONE');
#3127 = PRODUCT_DEFINITION_CONTEXT ( 'detailed design', #17969, 'design' ) ;
#3128 = CARTESIAN_POINT ( 'NONE',  ( 1.878215178125000939, 29.11562499938548498, 12.25316411605952283 ) ) ;
#3129 =( NAMED_UNIT ( * ) PLANE_ANGLE_UNIT ( ) SI_UNIT ( $, .RADIAN. ) );
#3130 = DIRECTION ( 'NONE',  ( -1.000000000000000000, 0.000000000000000000, 0.000000000000000000 ) ) ;
#3131 = DIRECTION ( 'NONE',  ( 1.000000000000000000, 0.000000000000000000, 0.000000000000000000 ) ) ;
#3132 = EDGE_CURVE ( 'NONE', #14371, #18149, #17208, .T. ) ;
#3133 = CARTESIAN_POINT ( 'NONE',  ( -16.66421332384646448, 26.25859848311288403, 1.000000000000000000 ) ) ;
#3134 = CARTESIAN_POINT ( 'NONE',  ( -3.756430356250002323, -27.46562499938548640, 11.16877607737301226 ) ) ;
#3135 = CARTESIAN_POINT ( 'NONE',  ( -1.878215178124998497, 25.55312499938548854, 12.25316411605951927 ) ) ;
#3136 = EDGE_CURVE ( 'NONE', #20975, #22395, #15113, .T. ) ;
#3137 = FACE_OUTER_BOUND ( 'NONE', #23201, .T. ) ;
#3138 = CARTESIAN_POINT ( 'NONE',  ( -1.999999999999998224, 26.14374999877096784, 12.46410161513774639 ) ) ;
#3139 = CARTESIAN_POINT ( 'NONE',  ( 3.015186248472646824, -29.84868090056883716, 11.64163568064553544 ) ) ;
#3140 = ORIENTED_EDGE ( 'NONE', *, *, #3029, .F. ) ;
#3141 = DIRECTION ( 'NONE',  ( 0.000000000000000000, 0.000000000000000000, 1.000000000000000000 ) ) ;
#3143 = ORIENTED_EDGE ( 'NONE', *, *, #12221, .T. ) ;
#3142 = DIRECTION ( 'NONE',  ( 0.000000000000000000, 0.000000000000000000, 1.000000000000000000 ) ) ;
#3144 = ADVANCED_FACE ( 'NONE', ( #15239 ), #5034, .F. ) ;
#3145 = ORIENTED_EDGE ( 'NONE', *, *, #21940, .T. ) ;
#3146 = ORIENTED_EDGE ( 'NONE', *, *, #18494, .T. ) ;
#3147 = EDGE_LOOP ( 'NONE', ( #22884, #22206 ) ) ;
#3148 = EDGE_LOOP ( 'NONE', ( #22343, #13600, #19888, #25002 ) ) ;
#3149 = DIRECTION ( 'NONE',  ( -0.000000000000000000, -1.000000000000000000, 0.000000000000000000 ) ) ;
#3150 = FACE_OUTER_BOUND ( 'NONE', #23571, .T. ) ;
#3151 = CARTESIAN_POINT ( 'NONE',  ( -3.756430356249996994, 28.62812499938548427, 8.999999999999992895 ) ) ;
#3152 = CARTESIAN_POINT ( 'NONE',  ( 1.878215178125000939, -12.25316411605952283, 4.678124999385483207 ) ) ;
#3153 = CARTESIAN_POINT ( 'NONE',  ( 2.000000000000000888, -12.46410161513774817, 1.218749998770966902 ) ) ;
#3154 = CARTESIAN_POINT ( 'NONE',  ( 3.756430356250002323, 26.56562499938548427, 11.16877607737301226 ) ) ;
#3155 = CARTESIAN_POINT ( 'NONE',  ( -22.56362157461193618, -13.02991752792603641, 20.00001200000000168 ) ) ;
#3156 = CARTESIAN_POINT ( 'NONE',  ( 4.000000000000003553, -8.999999999999992895, 0.4499999999999990119 ) ) ;
#3157 = CYLINDRICAL_SURFACE ( 'NONE', #25471, 4.000000000000000000 ) ;
#3158 = LINE ( 'NONE', #23170, #8697 ) ;
#3159 = CARTESIAN_POINT ( 'NONE',  ( -2.000000000000000888, -29.42500000000000071, 12.46410161513774817 ) ) ;
#3160 = DIRECTION ( 'NONE',  ( 0.000000000000000000, 0.000000000000000000, 1.000000000000000000 ) ) ;
#3161 = CYLINDRICAL_SURFACE ( 'NONE', #19229, 31.10000000000000142 ) ;
#3162 = EDGE_CURVE ( 'NONE', #23707, #2145, #4900, .T. ) ;
#3163 = DIRECTION ( 'NONE',  ( 0.000000000000000000, -0.000000000000000000, 1.000000000000000000 ) ) ;
#3164 = CARTESIAN_POINT ( 'NONE',  ( 30.63887302793244061, -5.335677986744896906, -6.500000000000000000 ) ) ;
#3165 = EDGE_LOOP ( 'NONE', ( #2913, #12994, #16862, #15874 ) ) ;
#3166 = ORIENTED_EDGE ( 'NONE', *, *, #20668, .T. ) ;
#3167 = ORIENTED_EDGE ( 'NONE', *, *, #10282, .F. ) ;
#3168 = CARTESIAN_POINT ( 'NONE',  ( 3.469446951953614189E-15, 39.50000000000000000, 8.999999999999992895 ) ) ;
#3169 = VERTEX_POINT ( 'NONE', #23204 ) ;
#3170 = AXIS2_PLACEMENT_3D ( 'NONE', #1060, #6577, #18619 ) ;
#3171 = CARTESIAN_POINT ( 'NONE',  ( -3.735045420075836212E-15, -26.26562499938548356, 4.662447845253954171 ) ) ;
#3172 = ORIENTED_EDGE ( 'NONE', *, *, #12772, .F. ) ;
#3173 = CARTESIAN_POINT ( 'NONE',  ( 29.41953157733093960, 10.08469938919488484, -6.500000000000000000 ) ) ;
#3174 = EDGE_CURVE ( 'NONE', #12039, #2722, #14972, .T. ) ;
#3175 = ORIENTED_EDGE ( 'NONE', *, *, #10574, .T. ) ;
#3176 = DIRECTION ( 'NONE',  ( -0.3090169943749382919, 0.9510565162951566398, 0.000000000000000000 ) ) ;
#3177 = CARTESIAN_POINT ( 'NONE',  ( 4.000000000000001776, 25.86250000000000071, 11.30940107675849760 ) ) ;
#3178 = CARTESIAN_POINT ( 'NONE',  ( -1.999999999999998224, 28.39374999877096784, 12.46410161513774639 ) ) ;
#3179 = DIRECTION ( 'NONE',  ( 1.000000000000000000, 0.000000000000000000, 0.000000000000000000 ) ) ;
#3180 = DIRECTION ( 'NONE',  ( -0.000000000000000000, -0.000000000000000000, -1.000000000000000000 ) ) ;
#3181 = CARTESIAN_POINT ( 'NONE',  ( 18.89079960070236908, 18.89079960070229802, 4.662447845253954171 ) ) ;
#3182 = CARTESIAN_POINT ( 'NONE',  ( 0.000000000000000000, 10.00000000000000000, 15.00000000000000178 ) ) ;
#3183 = CARTESIAN_POINT ( 'NONE',  ( 2.620986760973688460E-15, 25.78750000000000142, 13.61880215351699874 ) ) ;
#3184 = CARTESIAN_POINT ( 'NONE',  ( 19.87418373385361292, 17.21798635589416548, 5.746835883940462963 ) ) ;
#3185 = DIRECTION ( 'NONE',  ( -0.000000000000000000, -0.000000000000000000, 1.000000000000000000 ) ) ;
#3186 = VERTEX_POINT ( 'NONE', #21239 ) ;
#3187 = EDGE_LOOP ( 'NONE', ( #11686, #635 ) ) ;
#3188 = CARTESIAN_POINT ( 'NONE',  ( -3.999999999999999556, 27.45624999877097139, 11.30940107675849404 ) ) ;
#3189 = DIRECTION ( 'NONE',  ( 0.000000000000000000, 1.000000000000000000, 0.000000000000000000 ) ) ;
#3190 = CARTESIAN_POINT ( 'NONE',  ( 3.469446951953614189E-15, -8.999999999999992895, -10.00000000000000000 ) ) ;
#3191 = EDGE_CURVE ( 'NONE', #19876, #939, #20714, .T. ) ;
#3192 = CARTESIAN_POINT ( 'NONE',  ( -1.878215178124998497, 27.80312499938548498, 12.25316411605951927 ) ) ;
#3193 = LINE ( 'NONE', #23087, #19214 ) ;
#3194 = ORIENTED_EDGE ( 'NONE', *, *, #19749, .T. ) ;
#3195 = EDGE_LOOP ( 'NONE', ( #3439, #10877, #17181, #18667 ) ) ;
#3196 = CYLINDRICAL_SURFACE ( 'NONE', #12476, 31.10000000000000142 ) ;
#3197 = DIRECTION ( 'NONE',  ( -1.000000000000000000, 0.000000000000000000, 0.000000000000000000 ) ) ;
#3198 = ORIENTED_EDGE ( 'NONE', *, *, #6598, .T. ) ;
#3199 = CARTESIAN_POINT ( 'NONE',  ( 3.756430356249996105, -28.59062499938548640, 6.831223922626973533 ) ) ;
#3200 = ADVANCED_FACE ( 'NONE', ( #1892 ), #19521, .T. ) ;
#3201 = DIRECTION ( 'NONE',  ( 0.000000000000000000, -0.000000000000000000, 1.000000000000000000 ) ) ;
#3202 = CARTESIAN_POINT ( 'NONE',  ( 3.756430356250004987, 25.14062499938548356, 8.999999999999992895 ) ) ;
#3203 = CARTESIAN_POINT ( 'NONE',  ( -29.09636799667086748, -10.98232076577202676, 1.000000000000000000 ) ) ;
#3204 = CARTESIAN_POINT ( 'NONE',  ( -3.999999999999996447, 25.63750000000000284, 6.690598923241487306 ) ) ;
#3205 = CARTESIAN_POINT ( 'NONE',  ( 4.000000000000002665, 25.48750000000000426, 6.690598923241489970 ) ) ;
#3206 = APPLICATION_PROTOCOL_DEFINITION ( 'draft international standard', 'automotive_design', 1998, #19293 ) ;
#3207 = CARTESIAN_POINT ( 'NONE',  ( -11.44867358849371541, -28.91604871112453168, -6.500000000000000000 ) ) ;
#3208 = CARTESIAN_POINT ( 'NONE',  ( -25.16042852506104666, -18.28012134629567598, -6.500000000000000000 ) ) ;
#3209 = CARTESIAN_POINT ( 'NONE',  ( -3.756430356249997438, 27.65312499938548640, 11.16877607737301048 ) ) ;
#3210 = CARTESIAN_POINT ( 'NONE',  ( -3.795382382264993915, -29.75912104221810495, 7.710170883190207824 ) ) ;
#3211 = CARTESIAN_POINT ( 'NONE',  ( 18.23451611984813070, 18.23451611984806320, 13.61880215351699874 ) ) ;
#3212 = CARTESIAN_POINT ( 'NONE',  ( 19.23778763078571430, 16.58159025282627397, 5.746835883940462963 ) ) ;
#3213 = CARTESIAN_POINT ( 'NONE',  ( 19.24094079118243528, 20.75669031903440143, 4.999999999999992006 ) ) ;
#3214 = CARTESIAN_POINT ( 'NONE',  ( -1.878215178124998497, 27.24062499938548498, 12.25316411605951927 ) ) ;
#3215 = CARTESIAN_POINT ( 'NONE',  ( 0.000000000000000000, 0.000000000000000000, 0.000000000000000000 ) ) ;
#3216 = CARTESIAN_POINT ( 'NONE',  ( 18.25213002337956780, 20.90832740133887313, 12.25316411605951927 ) ) ;
#3217 = DIRECTION ( 'NONE',  ( 1.000000000000000000, 0.000000000000000000, 0.000000000000000000 ) ) ;
#3218 = ORIENTED_EDGE ( 'NONE', *, *, #9576, .T. ) ;
#3219 = CARTESIAN_POINT ( 'NONE',  ( 21.48720731330624645, 15.83035306381379748, 6.690598923241489970 ) ) ;
#3220 = CARTESIAN_POINT ( 'NONE',  ( 4.000000000000003553, 27.23124999877096997, 6.690598923241489970 ) ) ;
#3221 = CARTESIAN_POINT ( 'NONE',  ( -2.672651547586948120E-15, -29.07812499938548001, 13.33755215474602984 ) ) ;
#3223 = ORIENTED_EDGE ( 'NONE', *, *, #12704, .F. ) ;
#3222 = CYLINDRICAL_SURFACE ( 'NONE', #1662, 31.10000000000000142 ) ;
#3224 = CARTESIAN_POINT ( 'NONE',  ( -1.878215178124995832, 26.30312499938548498, 5.746835883940462963 ) ) ;
#3225 = EDGE_CURVE ( 'NONE', #14766, #18150, #17142, .T. ) ;
#3226 = ORIENTED_EDGE ( 'NONE', *, *, #16093, .T. ) ;
#3227 = CARTESIAN_POINT ( 'NONE',  ( -1.878215178125004048, -27.46562499938548640, 5.746835883940462963 ) ) ;
#3228 = VERTEX_POINT ( 'NONE', #17838 ) ;
#3229 = VERTEX_POINT ( 'NONE', #15748 ) ;
#3230 = EDGE_CURVE ( 'NONE', #2553, #22371, #12534, .T. ) ;
#3231 = CARTESIAN_POINT ( 'NONE',  ( 19.92166635246234563, 22.43180781836643689, 5.405792698933812979 ) ) ;
#3232 = CARTESIAN_POINT ( 'NONE',  ( 1.878215178125003382, 28.02812499938548996, 5.746835883940462963 ) ) ;
#3233 = LINE ( 'NONE', #17374, #9349 ) ;
#3234 = EDGE_CURVE ( 'NONE', #19968, #4306, #4187, .T. ) ;
#3235 = VECTOR ( 'NONE', #23585, 1000.000000000000000 ) ;
#3236 = FACE_OUTER_BOUND ( 'NONE', #8525, .T. ) ;
#3237 = CYLINDRICAL_SURFACE ( 'NONE', #9712, 0.5000000000000000000 ) ;
#3238 = FACE_OUTER_BOUND ( 'NONE', #21154, .T. ) ;
#3239 = CARTESIAN_POINT ( 'NONE',  ( 3.469446951953614189E-15, 30.00000000000000355, 8.999999999999992895 ) ) ;
#3240 = CARTESIAN_POINT ( 'NONE',  ( 3.756430356250002323, 28.25312499938548427, 11.16877607737301403 ) ) ;
#3241 = DIRECTION ( 'NONE',  ( -0.000000000000000000, -0.000000000000000000, -1.000000000000000000 ) ) ;
#3242 = CARTESIAN_POINT ( 'NONE',  ( -25.45105997952938637, -17.87326343783915306, -2.750000000000000000 ) ) ;
#3243 = DIRECTION ( 'NONE',  ( 1.000000000000000000, 0.000000000000000000, 0.000000000000000000 ) ) ;
#3244 = CARTESIAN_POINT ( 'NONE',  ( -1.999999999999998224, 27.55000000000000071, 12.46410161513774639 ) ) ;
#3245 = CARTESIAN_POINT ( 'NONE',  ( 3.756430356249995661, -29.04062499938548569, 6.831223922626973533 ) ) ;
#3246 = DIRECTION ( 'NONE',  ( 0.000000000000000000, 0.000000000000000000, 1.000000000000000000 ) ) ;
#3247 = DIRECTION ( 'NONE',  ( -0.000000000000000000, -1.000000000000000000, -0.000000000000000000 ) ) ;
#3248 = CARTESIAN_POINT ( 'NONE',  ( 4.000000000000003553, -8.999999999999992895, 18.00000000000000000 ) ) ;
#3249 = CARTESIAN_POINT ( 'NONE',  ( 5.577813053751546416E-15, 25.73124999877096997, 12.99999999999999289 ) ) ;
#3250 = APPLICATION_CONTEXT ( 'automotive_design' ) ;
#3251 = ORIENTED_EDGE ( 'NONE', *, *, #15969, .T. ) ;
#3252 = CARTESIAN_POINT ( 'NONE',  ( 4.000000000000063061, -11.30940107675846207, 2.662499999999998757 ) ) ;
#3253 = LINE ( 'NONE', #20931, #8786 ) ;
#3255 = ORIENTED_EDGE ( 'NONE', *, *, #23050, .F. ) ;
#3254 = DIRECTION ( 'NONE',  ( 0.000000000000000000, 0.000000000000000000, 1.000000000000000000 ) ) ;
#3256 =( BOUNDED_CURVE ( )  B_SPLINE_CURVE ( 2, ( #24130, #6216, #10263, #14208, #18257, #2950, #20858, #16561, #21004 ),
 .UNSPECIFIED., .F., .F. ) 
 B_SPLINE_CURVE_WITH_KNOTS ( ( 3, 2, 2, 2, 3 ),
 ( 0.4750000000000000333, 0.4833333333333333370, 0.5000000000000000000, 0.5166666666666667185, 0.5250000000000000222 ),
 .UNSPECIFIED. ) 
 CURVE ( )  GEOMETRIC_REPRESENTATION_ITEM ( )  RATIONAL_B_SPLINE_CURVE ( ( 0.9330127018922194093, 0.9330127018922196314, 1.000000000000000000, 0.8660254037844387076, 1.000000000000000000, 0.8660254037844387076, 1.000000000000000000, 0.9330127018922194093, 0.9330127018922194093 ) ) 
 REPRESENTATION_ITEM ( '' )  );
#3257 = ORIENTED_EDGE ( 'NONE', *, *, #16568, .T. ) ;
#3258 = VERTEX_POINT ( 'NONE', #13653 ) ;
#3259 = VERTEX_POINT ( 'NONE', #7889 ) ;
#3260 = VERTEX_POINT ( 'NONE', #25807 ) ;
#3261 = CARTESIAN_POINT ( 'NONE',  ( 21.21320343559646915, 21.21320343559638744, 8.999999999999992895 ) ) ;
#3262 =( BOUNDED_CURVE ( )  B_SPLINE_CURVE ( 2, ( #24709, #8751, #14781, #12546, #16879, #7183, #4715, #6799, #4833 ),
 .UNSPECIFIED., .F., .F. ) 
 B_SPLINE_CURVE_WITH_KNOTS ( ( 3, 2, 2, 2, 3 ),
 ( 0.5250000000000000222, 0.5333333333333333259, 0.5500000000000000444, 0.5666666666666666519, 0.5750000000000000666 ),
 .UNSPECIFIED. ) 
 CURVE ( )  GEOMETRIC_REPRESENTATION_ITEM ( )  RATIONAL_B_SPLINE_CURVE ( ( 0.9330127018922194093, 0.9330127018922194093, 1.000000000000000000, 0.8660254037844387076, 1.000000000000000000, 0.8660254037844387076, 1.000000000000000000, 0.9330127018922189652, 0.9330127018922194093 ) ) 
 REPRESENTATION_ITEM ( '' )  );
#3263 = CARTESIAN_POINT ( 'NONE',  ( 1.859271017917182139E-15, 29.33124999877096428, 12.99999999999999289 ) ) ;
#3264 = CIRCLE ( 'NONE', #23719, 0.5000000000000013323 ) ;
#3265 = EDGE_CURVE ( 'NONE', #13534, #6671, #7964, .T. ) ;
#3266 = CARTESIAN_POINT ( 'NONE',  ( 0.000000000000000000, 0.000000000000000000, -6.500000000000000000 ) ) ;
#3267 = EDGE_CURVE ( 'NONE', #24971, #8379, #10211, .T. ) ;
#3268 = CARTESIAN_POINT ( 'NONE',  ( 3.756430356250003655, -8.999999999999992895, 1.490624999385483429 ) ) ;
#3269 = CARTESIAN_POINT ( 'NONE',  ( 4.000000000000001776, -11.30940107675849760, 0.8062499987709654814 ) ) ;
#3270 = SURFACE_STYLE_USAGE ( .BOTH. , #1455 ) ;
#3271 = CARTESIAN_POINT ( 'NONE',  ( 3.756430356250003655, 26.15312499938548640, 8.999999999999992895 ) ) ;
#3272 = CARTESIAN_POINT ( 'NONE',  ( 27.49048467073858859, 14.54246377227349463, -6.500000000000000000 ) ) ;
#3273 = CIRCLE ( 'NONE', #9957, 0.4999999999999991118 ) ;
#3274 = DIRECTION ( 'NONE',  ( -0.000000000000000000, 0.000000000000000000, 1.000000000000000000 ) ) ;
#3275 = CARTESIAN_POINT ( 'NONE',  ( 4.000000000000003553, -6.690598923241489970, 0.03749999999999697325 ) ) ;
#3276 = CIRCLE ( 'NONE', #24576, 0.5000000000000001110 ) ;
#3277 = DIRECTION ( 'NONE',  ( 0.000000000000000000, 0.000000000000000000, 1.000000000000000000 ) ) ;
#3278 = DIRECTION ( 'NONE',  ( 0.000000000000000000, 0.000000000000000000, 1.000000000000000000 ) ) ;
#3279 = CARTESIAN_POINT ( 'NONE',  ( 30.78811501957144969, 4.393401135981008565, -6.500000000000000000 ) ) ;
#3280 = CARTESIAN_POINT ( 'NONE',  ( -3.752267015613588906E-15, -27.75624999877096855, 4.381197846482986158 ) ) ;
#3281 = CARTESIAN_POINT ( 'NONE',  ( 2.000000000000003997, -5.535898384862238508, 0.4687499987709661808 ) ) ;
#3282 = AXIS2_PLACEMENT_3D ( 'NONE', #23179, #20968, #8801 ) ;
#3283 = CARTESIAN_POINT ( 'NONE',  ( -1.999999999999996669, 25.15000000000000568, 5.535898384862237620 ) ) ;
#3284 = VECTOR ( 'NONE', #7814, 1000.000000000000000 ) ;
#3285 = DIRECTION ( 'NONE',  ( 0.000000000000000000, 0.000000000000000000, 1.000000000000000000 ) ) ;
#3286 = ORIENTED_EDGE ( 'NONE', *, *, #20421, .T. ) ;
#3287 = CARTESIAN_POINT ( 'NONE',  ( -1.859271017917182139E-15, -28.93749999999999645, 12.99999999999999289 ) ) ;
#3288 = VERTEX_POINT ( 'NONE', #11940 ) ;
#3289 = ORIENTED_EDGE ( 'NONE', *, *, #3082, .F. ) ;
#3290 = CYLINDRICAL_SURFACE ( 'NONE', #18369, 0.5000000000000004441 ) ;
#3291 = VERTEX_POINT ( 'NONE', #23465 ) ;
#3292 = CARTESIAN_POINT ( 'NONE',  ( 3.756430356249997882, -28.66562499938548569, 11.16877607737301226 ) ) ;
#3293 = ORIENTED_EDGE ( 'NONE', *, *, #14907, .T. ) ;
#3294 = CARTESIAN_POINT ( 'NONE',  ( 1.071796769724492338, 26.70759618943233704, 12.99999999999999467 ) ) ;
#3295 = AXIS2_PLACEMENT_3D ( 'NONE', #7997, #21983, #12029 ) ;
#3296 = EDGE_CURVE ( 'NONE', #6423, #8768, #15495, .T. ) ;
#3297 = VERTEX_POINT ( 'NONE', #17715 ) ;
#3298 = CARTESIAN_POINT ( 'NONE',  ( -3.999999999999996447, 27.92500000000000071, 8.999999999999992895 ) ) ;
#3299 = CARTESIAN_POINT ( 'NONE',  ( 0.000000000000000000, 0.000000000000000000, -6.500000000000000000 ) ) ;
#3301 = EDGE_CURVE ( 'NONE', #4358, #4649, #25300, .T. ) ;
#3300 = CIRCLE ( 'NONE', #7907, 31.10000000000000142 ) ;
#3302 = CIRCLE ( 'NONE', #17925, 0.4999999999999996114 ) ;
#3303 = CYLINDRICAL_SURFACE ( 'NONE', #18438, 0.5000000000000004441 ) ;
#3304 = DIRECTION ( 'NONE',  ( -0.000000000000000000, -1.000000000000000000, -0.000000000000000000 ) ) ;
#3305 = CARTESIAN_POINT ( 'NONE',  ( 15.96943717979804056, 21.28183193571671694, 6.831223922626973533 ) ) ;
#3306 = DIRECTION ( 'NONE',  ( -0.000000000000000000, -0.000000000000000000, 1.000000000000000000 ) ) ;
#3307 = CARTESIAN_POINT ( 'NONE',  ( -3.756430356249996994, 29.41562499938548569, 8.999999999999992895 ) ) ;
#3308 = CIRCLE ( 'NONE', #17942, 0.5000000000000007772 ) ;
#3309 = ADVANCED_FACE ( 'NONE', ( #15355 ), #17448, .T. ) ;
#3310 = CARTESIAN_POINT ( 'NONE',  ( 17.05888733012726632, 19.71508470808657520, 12.25316411605951927 ) ) ;
#3311 = DIRECTION ( 'NONE',  ( 0.000000000000000000, 0.000000000000000000, 1.000000000000000000 ) ) ;
#3312 = ORIENTED_EDGE ( 'NONE', *, *, #11200, .F. ) ;
#3313 = EDGE_LOOP ( 'NONE', ( #412, #21152, #3951, #4447 ) ) ;
#3314 = CARTESIAN_POINT ( 'NONE',  ( 0.000000000000000000, 27.98124999877096997, 13.61880215351699874 ) ) ;
#3316 = CARTESIAN_POINT ( 'NONE',  ( -10.98232076577180649, 29.09636799667095630, -6.500000000000000000 ) ) ;
#3315 = VECTOR ( 'NONE', #12743, 1000.000000000000000 ) ;
#3317 = ORIENTED_EDGE ( 'NONE', *, *, #16237, .T. ) ;
#3318 = CARTESIAN_POINT ( 'NONE',  ( -3.397863563849436108, 30.85476721088031482, -6.500000000000000000 ) ) ;
#3319 = VECTOR ( 'NONE', #23736, 1000.000000000000000 ) ;
#3320 = CARTESIAN_POINT ( 'NONE',  ( 1.878215178125000939, 28.32812499938548711, 12.25316411605952283 ) ) ;
#3321 = DIRECTION ( 'NONE',  ( 0.000000000000000000, 0.000000000000000000, -1.000000000000000000 ) ) ;
#3322 = EDGE_LOOP ( 'NONE', ( #21033, #9702, #24347, #10136 ) ) ;
#3323 = VERTEX_POINT ( 'NONE', #1498 ) ;
#3324 = CARTESIAN_POINT ( 'NONE',  ( 0.000000000000000000, 0.000000000000000000, -6.500000000000000000 ) ) ;
#3325 = VECTOR ( 'NONE', #6932, 1000.000000000000000 ) ;
#3326 = ORIENTED_EDGE ( 'NONE', *, *, #21610, .F. ) ;
#3327 = CARTESIAN_POINT ( 'NONE',  ( -2.672651547586948120E-15, -28.74062499938548854, 13.33755215474603162 ) ) ;
#3328 = EDGE_CURVE ( 'NONE', #23126, #8456, #20923, .T. ) ;
#3329 = CARTESIAN_POINT ( 'NONE',  ( 3.756430356250003655, 25.59062499938548285, 8.999999999999992895 ) ) ;
#3330 = CARTESIAN_POINT ( 'NONE',  ( 3.756430356250004987, 26.49062499938548854, 8.999999999999992895 ) ) ;
#3331 = CIRCLE ( 'NONE', #21294, 5.500000000000000000 ) ;
#3332 = CIRCLE ( 'NONE', #17122, 0.4999999999999999445 ) ;
#3333 = CARTESIAN_POINT ( 'NONE',  ( -4.000000000000003553, -26.33124999877097139, 6.690598923241489970 ) ) ;
#3334 = CARTESIAN_POINT ( 'NONE',  ( -3.756430356249996105, 29.37812499938548427, 6.831223922626973533 ) ) ;
#3335 = EDGE_CURVE ( 'NONE', #23467, #22705, #5522, .T. ) ;
#3336 = FACE_OUTER_BOUND ( 'NONE', #16051, .T. ) ;
#3337 = PRODUCT_CONTEXT ( 'NONE', #16627, 'mechanical' ) ;
#3338 = DIRECTION ( 'NONE',  ( 0.000000000000000000, 0.000000000000000000, 1.000000000000000000 ) ) ;
#3339 = EDGE_CURVE ( 'NONE', #1770, #13208, #5711, .T. ) ;
#3340 = DIRECTION ( 'NONE',  ( 0.000000000000000000, 0.000000000000000000, -1.000000000000000000 ) ) ;
#3341 = CARTESIAN_POINT ( 'NONE',  ( 1.878215178125000939, 25.96562499938548285, 12.25316411605952283 ) ) ;
#3342 = CIRCLE ( 'NONE', #3753, 0.5000000000000005551 ) ;
#3343 = CARTESIAN_POINT ( 'NONE',  ( 24.27856662945507438, 19.43607991388980238, -6.500000000000000000 ) ) ;
#3344 = CARTESIAN_POINT ( 'NONE',  ( 17.82559248041273037, 23.13798723633140142, 8.999999999999992895 ) ) ;
#3345 = CARTESIAN_POINT ( 'NONE',  ( 19.18020767368691182, 21.83640505164621004, 5.746835883940462963 ) ) ;
#3346 = CARTESIAN_POINT ( 'NONE',  ( -3.526711513754876570, 31.50000000000000000, 4.145898033750337497 ) ) ;
#3347 = CARTESIAN_POINT ( 'NONE',  ( 2.672651547586948120E-15, 26.82812499938548356, 13.33755215474602984 ) ) ;
#3348 = VECTOR ( 'NONE', #18603, 1000.000000000000000 ) ;
#3349 = CARTESIAN_POINT ( 'NONE',  ( 1.500000000000001776, -7.499999999999993783, 4.999999999999993783 ) ) ;
#3350 = VECTOR ( 'NONE', #7404, 1000.000000000000000 ) ;
#3351 = CARTESIAN_POINT ( 'NONE',  ( 17.48087792458429135, 22.79327268050296240, 6.831223922626973533 ) ) ;
#3352 = CARTESIAN_POINT ( 'NONE',  ( 21.22646168687465007, 18.39803456212839450, 12.46410161513774817 ) ) ;
#3353 = ORIENTED_EDGE ( 'NONE', *, *, #24202, .T. ) ;
#3354 = CARTESIAN_POINT ( 'NONE',  ( -3.999999999999996447, 25.61874999877096926, 8.999999999999992895 ) ) ;
#3355 = CARTESIAN_POINT ( 'NONE',  ( -3.999999999999996447, 29.21874999877096712, 8.999999999999992895 ) ) ;
#3356 = CARTESIAN_POINT ( 'NONE',  ( 3.756430356249995661, -28.47812499938548569, 6.831223922626973533 ) ) ;
#3358 = ORIENTED_EDGE ( 'NONE', *, *, #16174, .T. ) ;
#3357 = DIRECTION ( 'NONE',  ( 1.000000000000000000, -0.000000000000000000, -0.000000000000000000 ) ) ;
#3359 = CARTESIAN_POINT ( 'NONE',  ( -1.878215178124998497, 26.90312499938548285, 12.25316411605951927 ) ) ;
#3360 = EDGE_LOOP ( 'NONE', ( #7856, #5830, #23652, #3251 ) ) ;
#3361 = CARTESIAN_POINT ( 'NONE',  ( -3.756430356250003655, -28.29062499938548569, 8.999999999999992895 ) ) ;
#3362 = ORIENTED_EDGE ( 'NONE', *, *, #11269, .T. ) ;
#3363 = EDGE_LOOP ( 'NONE', ( #4654, #16710, #12568, #23853 ) ) ;
#3364 = CYLINDRICAL_SURFACE ( 'NONE', #12647, 31.10000000000000142 ) ;
#3365 = CARTESIAN_POINT ( 'NONE',  ( 2.003086131649545506E-15, 26.94062499938549138, 13.33755215474602984 ) ) ;
#3366 = AXIS2_PLACEMENT_3D ( 'NONE', #19560, #6094, #20081 ) ;
#3367 = CARTESIAN_POINT ( 'NONE',  ( -3.756430356249997438, -11.16877607737301048, 1.303124999385484095 ) ) ;
#3368 = VECTOR ( 'NONE', #536, 1000.000000000000000 ) ;
#3369 = AXIS2_PLACEMENT_3D ( 'NONE', #16247, #24085, #4343 ) ;
#3370 = EDGE_CURVE ( 'NONE', #25139, #13400, #22582, .T. ) ;
#3371 = CARTESIAN_POINT ( 'NONE',  ( -3.756430356249997882, -11.16877607737301226, 4.115624999385481431 ) ) ;
#3372 = CARTESIAN_POINT ( 'NONE',  ( 1.071796769724490117, -27.32634618820330630, 4.999999999999992895 ) ) ;
#3373 = AXIS2_PLACEMENT_3D ( 'NONE', #11351, #17494, #19332 ) ;
#3374 = EDGE_CURVE ( 'NONE', #4582, #7827, #4205, .T. ) ;
#3375 = CARTESIAN_POINT ( 'NONE',  ( 1.071796769724487675, 29.14240381056766793, 4.999999999999988454 ) ) ;
#3376 = CARTESIAN_POINT ( 'NONE',  ( 3.878215178125003604, 25.32343749907822783, 8.999999999999992895 ) ) ;
#3377 = CARTESIAN_POINT ( 'NONE',  ( -22.17092431280563503, 21.28941499438250062, -6.500000000000000000 ) ) ;
#3378 = CARTESIAN_POINT ( 'NONE',  ( 1.071796769724494336, 25.75134618820330346, 12.99999999999999467 ) ) ;
#3379 = DIRECTION ( 'NONE',  ( 0.000000000000000000, 0.000000000000000000, 1.000000000000000000 ) ) ;
#3380 = DIRECTION ( 'NONE',  ( 0.000000000000000000, 0.000000000000000000, 1.000000000000000000 ) ) ;
#3381 = CARTESIAN_POINT ( 'NONE',  ( 5.751896526290533274, 38.59087187958030540, 7.645898033760228252 ) ) ;
#3382 = CARTESIAN_POINT ( 'NONE',  ( 1.878215178124998497, -29.60312499938548569, 12.25316411605951927 ) ) ;
#3383 = CARTESIAN_POINT ( 'NONE',  ( 19.33184475599137642, 20.84759428384334612, 12.99999999999999645 ) ) ;
#3384 = FACE_OUTER_BOUND ( 'NONE', #17340, .T. ) ;
#3385 = AXIS2_PLACEMENT_3D ( 'NONE', #11697, #1777, #16026 ) ;
#3386 = FACE_OUTER_BOUND ( 'NONE', #11409, .T. ) ;
#3387 = LINE ( 'NONE', #25239, #4733 ) ;
#3388 = ORIENTED_EDGE ( 'NONE', *, *, #14330, .F. ) ;
#3389 = LINE ( 'NONE', #25356, #15108 ) ;
#3390 = EDGE_CURVE ( 'NONE', #17006, #10323, #14246, .T. ) ;
#3391 = CARTESIAN_POINT ( 'NONE',  ( -27.49048467073837898, 14.54246377227389075, -6.500000000000000000 ) ) ;
#3393 = EDGE_LOOP ( 'NONE', ( #4729, #20675, #20171, #8284 ) ) ;
#3392 = CARTESIAN_POINT ( 'NONE',  ( 0.000000000000000000, 0.000000000000000000, 1.000000000000000000 ) ) ;
#3394 = AXIS2_PLACEMENT_3D ( 'NONE', #8989, #24422, #6499 ) ;
#3395 = AXIS2_PLACEMENT_3D ( 'NONE', #1677, #25474, #19072 ) ;
#3396 = ORIENTED_EDGE ( 'NONE', *, *, #7684, .T. ) ;
#3397 = VERTEX_POINT ( 'NONE', #4480 ) ;
#3398 = VERTEX_POINT ( 'NONE', #20302 ) ;
#3399 = EDGE_LOOP ( 'NONE', ( #23435, #8641, #417, #23627 ) ) ;
#3400 = DIRECTION ( 'NONE',  ( 1.000000000000000000, 0.000000000000000000, 0.000000000000000000 ) ) ;
#3401 = CARTESIAN_POINT ( 'NONE',  ( -3.999999999999996447, 29.21874999877096712, 8.999999999999992895 ) ) ;
#3402 = EDGE_CURVE ( 'NONE', #17275, #16647, #24435, .T. ) ;
#3403 = CARTESIAN_POINT ( 'NONE',  ( 5.577813053751546416E-15, 27.81250000000000355, 4.999999999999992006 ) ) ;
#3404 = AXIS2_PLACEMENT_3D ( 'NONE', #10880, #15085, #20428 ) ;
#3405 = CARTESIAN_POINT ( 'NONE',  ( -3.756430356249995661, -6.831223922626973533, 1.228124999385478144 ) ) ;
#3406 = CARTESIAN_POINT ( 'NONE',  ( -1.999999999999998224, -12.46410161513774639, 1.593749998770967125 ) ) ;
#3407 =( LENGTH_UNIT ( ) NAMED_UNIT ( * ) SI_UNIT ( .MILLI., .METRE. ) );
#3408 = CARTESIAN_POINT ( 'NONE',  ( 1.878215178125000939, 26.07812499938548356, 12.25316411605952283 ) ) ;
#3409 = DIRECTION ( 'NONE',  ( 1.000000000000000000, 0.000000000000000000, 0.000000000000000000 ) ) ;
#3410 = CARTESIAN_POINT ( 'NONE',  ( 2.000000000000000888, 28.46874999877097068, 12.46410161513774817 ) ) ;
#3411 = CARTESIAN_POINT ( 'NONE',  ( -3.999999999999997335, -11.30940107675849404, 0.7124999999999986899 ) ) ;
#3412 = CIRCLE ( 'NONE', #21782, 24.00000000000000355 ) ;
#3413 = LINE ( 'NONE', #11515, #13794 ) ;
#3414 = CYLINDRICAL_SURFACE ( 'NONE', #19130, 24.00000000000000355 ) ;
#3415 = FACE_OUTER_BOUND ( 'NONE', #24009, .T. ) ;
#3416 = EDGE_CURVE ( 'NONE', #9389, #1951, #35, .T. ) ;
#3417 =( BOUNDED_CURVE ( )  B_SPLINE_CURVE ( 2, ( #11522, #11646, #23427, #19372, #9557, #5642, #24779 ),
 .UNSPECIFIED., .F., .F. ) 
 B_SPLINE_CURVE_WITH_KNOTS ( ( 3, 2, 2, 3 ),
 ( 0.9500000000000003997, 0.9666666666666670071, 0.9833333333333333925, 1.000000000000000000 ),
 .UNSPECIFIED. ) 
 CURVE ( )  GEOMETRIC_REPRESENTATION_ITEM ( )  RATIONAL_B_SPLINE_CURVE ( ( 0.9999999999999964473, 0.8660254037844422603, 1.000000000000000000, 0.8660254037844387076, 1.000000000000000000, 0.8660254037844387076, 1.000000000000000000 ) ) 
 REPRESENTATION_ITEM ( '' )  );
#3418 = CARTESIAN_POINT ( 'NONE',  ( 3.999999999999996447, -26.51874999877097139, 8.999999999999992895 ) ) ;
#3419 = CIRCLE ( 'NONE', #21787, 26.00000000000000711 ) ;
#3420 = CARTESIAN_POINT ( 'NONE',  ( -1.878215178124998497, -12.25316411605951927, 3.703124999385482674 ) ) ;
#3421 = CARTESIAN_POINT ( 'NONE',  ( -10.94867358849309547, 28.91604871112477326, -6.500000000000000000 ) ) ;
#3422 = CARTESIAN_POINT ( 'NONE',  ( -15.41874213889433776, -27.00874656207289704, -2.750000000000000000 ) ) ;
#3423 = CARTESIAN_POINT ( 'NONE',  ( -1.859271017917182139E-15, -25.78750000000000142, 12.99999999999999289 ) ) ;
#3424 = ORIENTED_EDGE ( 'NONE', *, *, #12800, .F. ) ;
#3425 = EDGE_CURVE ( 'NONE', #9259, #14853, #11294, .T. ) ;
#3426 = CARTESIAN_POINT ( 'NONE',  ( 5.335677986744788548, 30.63887302793246548, -2.750000000000000000 ) ) ;
#3427 = VERTEX_POINT ( 'NONE', #584 ) ;
#3428 =( BOUNDED_CURVE ( )  B_SPLINE_CURVE ( 2, ( #11248, #23167, #3410, #17157, #19612, #3540, #19228, #1458, #9429 ),
 .UNSPECIFIED., .F., .F. ) 
 B_SPLINE_CURVE_WITH_KNOTS ( ( 3, 2, 2, 2, 3 ),
 ( 0.6750000000000000444, 0.6833333333333333481, 0.6999999999999999556, 0.7166666666666666741, 0.7249999999999999778 ),
 .UNSPECIFIED. ) 
 CURVE ( )  GEOMETRIC_REPRESENTATION_ITEM ( )  RATIONAL_B_SPLINE_CURVE ( ( 0.9330127018922194093, 0.9330127018922198534, 1.000000000000000000, 0.8660254037844387076, 1.000000000000000000, 0.8660254037844387076, 1.000000000000000000, 0.9330127018922194093, 0.9330127018922194093 ) ) 
 REPRESENTATION_ITEM ( '' )  );
#3429 = EDGE_CURVE ( 'NONE', #3297, #4579, #8394, .T. ) ;
#3430 = AXIS2_PLACEMENT_3D ( 'NONE', #5908, #13895, #20015 ) ;
#3431 = ORIENTED_EDGE ( 'NONE', *, *, #4672, .F. ) ;
#3432 = CYLINDRICAL_SURFACE ( 'NONE', #11683, 8.000000000000000000 ) ;
#3433 = ORIENTED_EDGE ( 'NONE', *, *, #22465, .T. ) ;
#3434 = CARTESIAN_POINT ( 'NONE',  ( -2.672651547586948120E-15, -28.29062499938548569, 13.33755215474602984 ) ) ;
#3435 = ORIENTED_EDGE ( 'NONE', *, *, #14268, .F. ) ;
#3436 = CARTESIAN_POINT ( 'NONE',  ( 4.000000000000001776, 26.76250000000000284, 11.30940107675849760 ) ) ;
#3437 = AXIS2_PLACEMENT_3D ( 'NONE', #17377, #11597, #5215 ) ;
#3438 = VECTOR ( 'NONE', #917, 999.9999999999998863 ) ;
#3439 = ORIENTED_EDGE ( 'NONE', *, *, #16353, .F. ) ;
#3440 = CIRCLE ( 'NONE', #1355, 0.5000000000000006661 ) ;
#3441 = CARTESIAN_POINT ( 'NONE',  ( 2.000000000000003997, 28.22500000000000142, 5.535898384862238508 ) ) ;
#3442 = DIRECTION ( 'NONE',  ( 0.000000000000000000, -0.000000000000000000, 1.000000000000000000 ) ) ;
#3443 = CARTESIAN_POINT ( 'NONE',  ( -31.10000000000000142, 3.257552089140643357E-13, -6.500000000000000000 ) ) ;
#3444 = CARTESIAN_POINT ( 'NONE',  ( 3.469446951953614189E-15, 30.00000000000000355, 8.999999999999992895 ) ) ;
#3445 = CARTESIAN_POINT ( 'NONE',  ( 19.47643616943617317, 16.82023879147673284, 5.746835883940462963 ) ) ;
#3446 = CARTESIAN_POINT ( 'NONE',  ( 3.469446951953614189E-15, 25.00000000000000000, 4.999999999999992006 ) ) ;
#3447 = CARTESIAN_POINT ( 'NONE',  ( -3.999999999999997335, 26.61250000000000071, 11.30940107675849404 ) ) ;
#3448 = AXIS2_PLACEMENT_3D ( 'NONE', #24195, #6806, #16368 ) ;
#3449 = CARTESIAN_POINT ( 'NONE',  ( 16.02247018838703241, 21.33486494430571412, 11.16877607737301048 ) ) ;
#3450 = DIRECTION ( 'NONE',  ( 0.000000000000000000, 0.000000000000000000, 1.000000000000000000 ) ) ;
#3451 = ORIENTED_EDGE ( 'NONE', *, *, #23269, .T. ) ;
#3452 = EDGE_CURVE ( 'NONE', #10325, #4475, #14652, .T. ) ;
#3453 = ORIENTED_EDGE ( 'NONE', *, *, #12991, .T. ) ;
#3454 = CARTESIAN_POINT ( 'NONE',  ( 2.000000000000005329, 28.16874999877097352, 5.535898384862238508 ) ) ;
#3456 = EDGE_CURVE ( 'NONE', #24553, #20362, #14318, .T. ) ;
#3455 = CARTESIAN_POINT ( 'NONE',  ( -3.735045420075836212E-15, -29.30312499938548498, 4.662447845253954171 ) ) ;
#3457 = ORIENTED_EDGE ( 'NONE', *, *, #19557, .T. ) ;
#3458 = DIRECTION ( 'NONE',  ( -0.000000000000000000, -1.000000000000000000, -0.000000000000000000 ) ) ;
#3459 = CARTESIAN_POINT ( 'NONE',  ( -1.878215178124998497, 27.35312499938548569, 12.25316411605951927 ) ) ;
#3460 = DIRECTION ( 'NONE',  ( -0.9510565162951561957, -0.3090169943749392911, 0.000000000000000000 ) ) ;
#3461 = EDGE_LOOP ( 'NONE', ( #4451, #3737, #12560, #12370 ) ) ;
#3462 = VERTEX_POINT ( 'NONE', #22922 ) ;
#3463 = CARTESIAN_POINT ( 'NONE',  ( 18.35384038830430597, 18.35384038830423492, 4.999999999999992006 ) ) ;
#3464 = EDGE_CURVE ( 'NONE', #16823, #12173, #7549, .T. ) ;
#3465 = AXIS2_PLACEMENT_3D ( 'NONE', #21629, #2154, #17589 ) ;
#3466 = CYLINDRICAL_SURFACE ( 'NONE', #20703, 31.10000000000000142 ) ;
#3467 = ORIENTED_EDGE ( 'NONE', *, *, #2794, .T. ) ;
#3468 = CARTESIAN_POINT ( 'NONE',  ( -1.071796769724487230, 25.58259618943233704, 4.999999999999992006 ) ) ;
#3469 = CARTESIAN_POINT ( 'NONE',  ( -3.756430356249997882, 25.40312499938548285, 11.16877607737301226 ) ) ;
#3470 = CARTESIAN_POINT ( 'NONE',  ( 4.006172263299091013E-15, 28.17812499938548498, 13.33755215474603162 ) ) ;
#3471 = VECTOR ( 'NONE', #23774, 1000.000000000000000 ) ;
#3472 = CARTESIAN_POINT ( 'NONE',  ( 4.648177544792955347E-16, 25.78750000000000497, 12.99999999999999289 ) ) ;
#3473 = CARTESIAN_POINT ( 'NONE',  ( 4.000000000000002665, 27.28749999999999787, 6.690598923241489970 ) ) ;
#3474 = VECTOR ( 'NONE', #11414, 1000.000000000000000 ) ;
#3475 = DIRECTION ( 'NONE',  ( 0.000000000000000000, 0.000000000000000000, 1.000000000000000000 ) ) ;
#3476 = CARTESIAN_POINT ( 'NONE',  ( -1.453535542772161238, 31.06601413805604750, -2.750000000000000000 ) ) ;
#3477 = CIRCLE ( 'NONE', #21463, 0.4999999999999995004 ) ;
#3478 = CARTESIAN_POINT ( 'NONE',  ( 3.735045420075836212E-15, 27.50312499938548427, 4.662447845253954171 ) ) ;
#3479 = DIRECTION ( 'NONE',  ( 0.8660254037844397068, 0.4999999999999983347, -0.000000000000000000 ) ) ;
#3480 = CARTESIAN_POINT ( 'NONE',  ( 18.78246010926947918, 21.43865748722877740, 5.746835883940462963 ) ) ;
#3481 = CARTESIAN_POINT ( 'NONE',  ( 16.97706434298888212, 22.28945909890755317, 11.16877607737301226 ) ) ;
#3482 = EDGE_CURVE ( 'NONE', #11943, #15750, #16792, .T. ) ;
#3483 = FACE_OUTER_BOUND ( 'NONE', #4356, .T. ) ;
#3484 = DIRECTION ( 'NONE',  ( 0.000000000000000000, -1.000000000000000000, 0.000000000000000000 ) ) ;
#3486 = ADVANCED_FACE ( 'NONE', ( #23059 ), #11019, .F. ) ;
#3485 = CARTESIAN_POINT ( 'NONE',  ( 21.21320343559646915, 21.21320343559638744, 4.999999999999992006 ) ) ;
#3487 = CARTESIAN_POINT ( 'NONE',  ( 17.16267987305034382, 22.47507462896901842, 6.831223922626973533 ) ) ;
#3488 = DIRECTION ( 'NONE',  ( 0.000000000000000000, 1.000000000000000000, 0.000000000000000000 ) ) ;
#3489 = ORIENTED_EDGE ( 'NONE', *, *, #4704, .T. ) ;
#3490 = DIRECTION ( 'NONE',  ( 1.000000000000000000, 0.000000000000000000, 0.000000000000000000 ) ) ;
#3491 = CARTESIAN_POINT ( 'NONE',  ( 1.878215178125004048, 26.67812499938548498, 5.746835883940462963 ) ) ;
#3492 = CARTESIAN_POINT ( 'NONE',  ( -4.000000000000003553, -25.93750000000000000, 6.690598923241489970 ) ) ;
#3494 = ORIENTED_EDGE ( 'NONE', *, *, #20508, .F. ) ;
#3493 = CARTESIAN_POINT ( 'NONE',  ( -3.756430356249996549, 25.44062499938548783, 6.831223922626973533 ) ) ;
#3495 = CARTESIAN_POINT ( 'NONE',  ( -1.859271017917182139E-15, -28.93749999999999645, 12.99999999999999289 ) ) ;
#3496 = COLOUR_RGB ( '',0.8941176470588234615, 0.8941176470588234615, 0.8941176470588234615 ) ;
#3497 = CARTESIAN_POINT ( 'NONE',  ( -17.18149551509903361, 19.58805710660143973, 20.00001200000000168 ) ) ;
#3498 = CARTESIAN_POINT ( 'NONE',  ( 1.878215178124995832, -28.89062499938548356, 5.746835883940462963 ) ) ;
#3499 = ORIENTED_EDGE ( 'NONE', *, *, #8418, .F. ) ;
#3500 = VERTEX_POINT ( 'NONE', #8669 ) ;
#3501 = CARTESIAN_POINT ( 'NONE',  ( 18.51824573262021190, 23.60264142991855252, 7.227341970420264161 ) ) ;
#3502 = CARTESIAN_POINT ( 'NONE',  ( 4.006172263299091013E-15, 25.70312499938548356, 4.662447845253954171 ) ) ;
#3503 = ADVANCED_FACE ( 'NONE', ( #2663 ), #10625, .F. ) ;
#3504 = CIRCLE ( 'NONE', #14787, 0.5000000000000013323 ) ;
#3505 = CARTESIAN_POINT ( 'NONE',  ( -1.878215178124995832, -5.746835883940462963, 1.640624999385484450 ) ) ;
#3506 = CARTESIAN_POINT ( 'NONE',  ( -3.756430356249997882, -11.16877607737301226, 3.665624999385481697 ) ) ;
#3507 = CYLINDRICAL_SURFACE ( 'NONE', #942, 0.5000000000000004441 ) ;
#3508 = B_SPLINE_CURVE_WITH_KNOTS ( 'NONE', 3,
 ( #25594, #11336, #5705, #21657, #5454, #25457, #9638, #13822, #15661, #25334, #1924, #21416, #1800, #17871, #11724, #9769, #23746, #9502, #5835, #13569, #9885, #25843, #11469, #21278, #3497, #5323, #9387, #13304, #7541, #17617, #15535, #23502, #5589, #21534 ),
 .UNSPECIFIED., .F., .F.,
 ( 4, 2, 2, 2, 2, 2, 2, 2, 2, 2, 2, 2, 2, 2, 2, 2, 4 ),
 ( 0.000000000000000000, 0.03124999999999998612, 0.06249999999999995837, 0.09374999999999993061, 0.1249999999999999029, 0.1562499999999998890, 0.1874999999999998890, 0.2187499999999998890, 0.2499999999999998890, 0.2812499999999998890, 0.3124999999999998890, 0.3437499999999998335, 0.3749999999999998335, 0.4062499999999998335, 0.4374999999999998335, 0.4687499999999998890, 0.5000000000000000000 ),
 .UNSPECIFIED. ) ;
#3509 = DIRECTION ( 'NONE',  ( 1.000000000000000000, 0.000000000000000000, 0.000000000000000000 ) ) ;
#3510 = STYLED_ITEM ( 'NONE', ( #5333 ), #16592 ) ;
#3511 = CARTESIAN_POINT ( 'NONE',  ( 4.000000000000003553, 28.63749999999999929, 6.690598923241489970 ) ) ;
#3512 = CARTESIAN_POINT ( 'NONE',  ( 1.859271017917182139E-15, 26.68750000000000000, 12.99999999999999289 ) ) ;
#3513 = LINE ( 'NONE', #17498, #11208 ) ;
#3514 = CARTESIAN_POINT ( 'NONE',  ( 18.67203843983824996, 18.67203843983817890, 4.381197846482986158 ) ) ;
#3515 = ORIENTED_EDGE ( 'NONE', *, *, #10429, .F. ) ;
#3516 = FACE_BOUND ( 'NONE', #24979, .T. ) ;
#3517 = LINE ( 'NONE', #9661, #8400 ) ;
#3518 = CARTESIAN_POINT ( 'NONE',  ( 1.878215178125004048, 26.67812499938548498, 5.746835883940462963 ) ) ;
#3519 = CARTESIAN_POINT ( 'NONE',  ( 1.859271017917182139E-15, 29.78124999877096712, 12.99999999999999289 ) ) ;
#3520 = CARTESIAN_POINT ( 'NONE',  ( 4.000000000000003553, 27.28749999999999787, 6.690598923241489970 ) ) ;
#3521 = CARTESIAN_POINT ( 'NONE',  ( 4.000000000000001776, 28.95624999877097494, 11.30940107675849760 ) ) ;
#3522 = ORIENTED_EDGE ( 'NONE', *, *, #3035, .F. ) ;
#3523 = CARTESIAN_POINT ( 'NONE',  ( -3.999999999999996447, -8.999999999999992895, 2.474999999999997868 ) ) ;
#3524 = CARTESIAN_POINT ( 'NONE',  ( -5.606865722240301331, 38.73198406056108922, 7.645898033750359701 ) ) ;
#3526 = ORIENTED_EDGE ( 'NONE', *, *, #14414, .T. ) ;
#3525 = CARTESIAN_POINT ( 'NONE',  ( -4.000000000000003553, -26.35000000000000142, 8.999999999999992895 ) ) ;
#3527 = ORIENTED_EDGE ( 'NONE', *, *, #21031, .T. ) ;
#3528 = ORIENTED_EDGE ( 'NONE', *, *, #3225, .T. ) ;
#3530 = ADVANCED_FACE ( 'NONE', ( #5147 ), #11696, .F. ) ;
#3529 = ORIENTED_EDGE ( 'NONE', *, *, #23959, .F. ) ;
#3531 = VERTEX_POINT ( 'NONE', #23628 ) ;
#3532 = DIRECTION ( 'NONE',  ( 0.000000000000000000, -0.000000000000000000, 1.000000000000000000 ) ) ;
#3533 = CARTESIAN_POINT ( 'NONE',  ( -3.169364099030547166, 38.99989214654019776, 13.49581827627000763 ) ) ;
#3534 = DIRECTION ( 'NONE',  ( 0.4817536741017131585, -0.8763066800438648052, 0.000000000000000000 ) ) ;
#3535 = CARTESIAN_POINT ( 'NONE',  ( 3.756430356250000546, 25.55312499938548498, 11.16877607737301226 ) ) ;
#3536 = CARTESIAN_POINT ( 'NONE',  ( -3.756430356249997882, -11.16877607737301226, 1.753124999385479832 ) ) ;
#3537 = CARTESIAN_POINT ( 'NONE',  ( 2.000000000000003997, -5.535898384862238508, 1.368749998770967702 ) ) ;
#3538 = CARTESIAN_POINT ( 'NONE',  ( -3.756430356249995661, 27.24062499938548498, 6.831223922626973533 ) ) ;
#3539 = DIRECTION ( 'NONE',  ( -0.000000000000000000, -0.000000000000000000, 1.000000000000000000 ) ) ;
#3540 = CARTESIAN_POINT ( 'NONE',  ( 4.000000000000003553, 28.58124999877096784, 6.690598923241489970 ) ) ;
#3541 = CARTESIAN_POINT ( 'NONE',  ( -1.999999999999998224, -12.46410161513774639, 2.100000000000000977 ) ) ;
#3542 = DIRECTION ( 'NONE',  ( 0.000000000000000000, 0.000000000000000000, 1.000000000000000000 ) ) ;
#3543 = FACE_OUTER_BOUND ( 'NONE', #14525, .T. ) ;
#3544 = LINE ( 'NONE', #9552, #2602 ) ;
#3545 = CARTESIAN_POINT ( 'NONE',  ( 3.999999999999996447, -27.41874999877096641, 8.999999999999992895 ) ) ;
#3546 = DIRECTION ( 'NONE',  ( 0.000000000000000000, 0.000000000000000000, 1.000000000000000000 ) ) ;
#3547 = FACE_OUTER_BOUND ( 'NONE', #7383, .T. ) ;
#3548 = CARTESIAN_POINT ( 'NONE',  ( -1.999999999999998224, 25.75000000000000355, 12.46410161513774639 ) ) ;
#3549 = ORIENTED_EDGE ( 'NONE', *, *, #4219, .T. ) ;
#3550 = ADVANCED_FACE ( 'NONE', ( #13955 ), #97, .F. ) ;
#3551 = DIRECTION ( 'NONE',  ( 0.000000000000000000, 0.000000000000000000, 1.000000000000000000 ) ) ;
#3552 = EDGE_LOOP ( 'NONE', ( #3048, #99, #5644, #20396 ) ) ;
#3553 = ORIENTED_EDGE ( 'NONE', *, *, #20988, .F. ) ;
#3554 = CARTESIAN_POINT ( 'NONE',  ( 21.21320343559646915, 21.21320343559638744, 8.999999999999992895 ) ) ;
#3555 = ORIENTED_EDGE ( 'NONE', *, *, #12503, .T. ) ;
#3556 = CARTESIAN_POINT ( 'NONE',  ( 3.756430356249996994, -28.62812499938548427, 8.999999999999992895 ) ) ;
#3557 = ORIENTED_EDGE ( 'NONE', *, *, #12840, .T. ) ;
#3558 = CARTESIAN_POINT ( 'NONE',  ( 1.859271017917182139E-15, 28.93749999999999645, 12.99999999999999289 ) ) ;
#3559 = ADVANCED_FACE ( 'NONE', ( #10014 ), #8070, .T. ) ;
#3560 = VERTEX_POINT ( 'NONE', #16050 ) ;
#3561 = EDGE_CURVE ( 'NONE', #11048, #8528, #9033, .T. ) ;
#3562 = CARTESIAN_POINT ( 'NONE',  ( -3.999999999999996003, 26.98750000000000426, 6.690598923241487306 ) ) ;
#3563 = CARTESIAN_POINT ( 'NONE',  ( 0.000000000000000000, 0.000000000000000000, -6.500000000000000000 ) ) ;
#3564 = VECTOR ( 'NONE', #12295, 1000.000000000000000 ) ;
#3565 = CARTESIAN_POINT ( 'NONE',  ( -3.756430356249995661, -6.831223922626973533, 0.8906249993854814528 ) ) ;
#3566 = DIRECTION ( 'NONE',  ( 0.000000000000000000, -1.000000000000000000, 0.000000000000000000 ) ) ;
#3567 = AXIS2_PLACEMENT_3D ( 'NONE', #14925, #8529, #12829 ) ;
#3568 = CARTESIAN_POINT ( 'NONE',  ( 18.22334004483017011, 23.53573480074883761, 8.999999999999992895 ) ) ;
#3569 = EDGE_CURVE ( 'NONE', #4968, #24375, #11725, .T. ) ;
#3570 =( BOUNDED_CURVE ( )  B_SPLINE_CURVE ( 2, ( #9009, #9269, #16988, #23134, #13191, #15404, #24954, #21162, #5090 ),
 .UNSPECIFIED., .F., .F. ) 
 B_SPLINE_CURVE_WITH_KNOTS ( ( 3, 2, 2, 2, 3 ),
 ( 0.7750000000000000222, 0.7833333333333333259, 0.8000000000000000444, 0.8166666666666666519, 0.8250000000000000666 ),
 .UNSPECIFIED. ) 
 CURVE ( )  GEOMETRIC_REPRESENTATION_ITEM ( )  RATIONAL_B_SPLINE_CURVE ( ( 0.9330127018922194093, 0.9330127018922194093, 1.000000000000000000, 0.8660254037844387076, 1.000000000000000000, 0.8660254037844387076, 1.000000000000000000, 0.9330127018922189652, 0.9330127018922194093 ) ) 
 REPRESENTATION_ITEM ( '' )  );
#3571 = CARTESIAN_POINT ( 'NONE',  ( 1.859271017917182139E-15, 27.08124999877096784, 12.99999999999999289 ) ) ;
#3572 = CARTESIAN_POINT ( 'NONE',  ( -1.999999999999995781, 26.50000000000000355, 5.535898384862237620 ) ) ;
#3573 =( BOUNDED_CURVE ( )  B_SPLINE_CURVE ( 2, ( #3523, #23653, #5731, #13711, #3774, #3252, #21829 ),
 .UNSPECIFIED., .F., .F. ) 
 B_SPLINE_CURVE_WITH_KNOTS ( ( 3, 2, 2, 3 ),
 ( 0.5499999999999997113, 0.5666666666666665408, 0.5833333333333335924, 0.6000000000000004219 ),
 .UNSPECIFIED. ) 
 CURVE ( )  GEOMETRIC_REPRESENTATION_ITEM ( )  RATIONAL_B_SPLINE_CURVE ( ( 1.000000000000002665, 0.8660254037844360431, 1.000000000000000000, 0.8660254037844387076, 1.000000000000000000, 0.8660254037844351549, 1.000000000000003553 ) ) 
 REPRESENTATION_ITEM ( '' )  );
#3574 = CARTESIAN_POINT ( 'NONE',  ( 17.56042743746777646, 22.87282219338644751, 6.831223922626973533 ) ) ;
#3575 = CARTESIAN_POINT ( 'NONE',  ( -1.859271017917182139E-15, -29.33124999877096428, 12.99999999999999289 ) ) ;
#3576 = AXIS2_PLACEMENT_3D ( 'NONE', #452, #24380, #8425 ) ;
#3577 = ORIENTED_EDGE ( 'NONE', *, *, #21161, .T. ) ;
#3578 = VERTEX_POINT ( 'NONE', #1664 ) ;
#3579 = CARTESIAN_POINT ( 'NONE',  ( 4.000000000000007105, 28.58124999877097139, 6.690598923241489970 ) ) ;
#3580 = EDGE_LOOP ( 'NONE', ( #5554, #4297, #3745, #11494 ) ) ;
#3581 = CARTESIAN_POINT ( 'NONE',  ( 0.5000000000000001110, 10.00000000000000000, 15.00000000000000178 ) ) ;
#3582 = CARTESIAN_POINT ( 'NONE',  ( 1.878215178125004048, 26.67812499938548498, 5.746835883940462963 ) ) ;
#3583 = DIRECTION ( 'NONE',  ( 0.000000000000000000, 0.000000000000000000, 1.000000000000000000 ) ) ;
#3584 = EDGE_LOOP ( 'NONE', ( #18839, #20354, #8024, #1431 ) ) ;
#3585 = ORIENTED_EDGE ( 'NONE', *, *, #24328, .F. ) ;
#3586 = PLANE ( 'NONE',  #14418 ) ;
#3587 = ORIENTED_EDGE ( 'NONE', *, *, #17336, .T. ) ;
#3588 = FACE_OUTER_BOUND ( 'NONE', #25625, .T. ) ;
#3589 = CARTESIAN_POINT ( 'NONE',  ( -1.878215178124995832, 25.29062499938548569, 5.746835883940462963 ) ) ;
#3590 = CARTESIAN_POINT ( 'NONE',  ( 1.878215178125001605, 27.76562499938548711, 12.25316411605952283 ) ) ;
#3591 = CYLINDRICAL_SURFACE ( 'NONE', #8823, 4.000000000000000000 ) ;
#3592 = CARTESIAN_POINT ( 'NONE',  ( -1.999999999999998224, 27.55000000000000426, 12.46410161513774639 ) ) ;
#3593 = ADVANCED_FACE ( 'NONE', ( #5590 ), #24012, .T. ) ;
#3594 = EDGE_CURVE ( 'NONE', #10718, #16937, #25595, .T. ) ;
#3595 = CARTESIAN_POINT ( 'NONE',  ( -3.756430356249996994, 29.41562499938548569, 8.999999999999992895 ) ) ;
#3596 = DIRECTION ( 'NONE',  ( 1.000000000000000000, 0.000000000000000000, 0.000000000000000000 ) ) ;
#3597 = EDGE_CURVE ( 'NONE', #5826, #3462, #21331, .T. ) ;
#3598 = DIRECTION ( 'NONE',  ( 1.000000000000000000, 0.000000000000000000, 0.000000000000000000 ) ) ;
#3599 = CARTESIAN_POINT ( 'NONE',  ( 3.756430356250003211, 27.87812499938548427, 6.831223922626973533 ) ) ;
#3600 = CARTESIAN_POINT ( 'NONE',  ( -3.472074595960224386, -29.79875828571876184, 6.996763648122163559 ) ) ;
#3601 = CARTESIAN_POINT ( 'NONE',  ( 16.57281518405975262, 22.22966943355206126, 6.690598923241487306 ) ) ;
#3602 = CARTESIAN_POINT ( 'NONE',  ( 23.03192121915348878, 17.71952646323466496, 11.16877607737301226 ) ) ;
#3603 = LINE ( 'NONE', #21403, #20510 ) ;
#3604 = CARTESIAN_POINT ( 'NONE',  ( 3.756430356250002323, 29.60312499938548569, 11.16877607737301226 ) ) ;
#3605 = CARTESIAN_POINT ( 'NONE',  ( 21.21320343559646915, 21.21320343559638744, 8.999999999999992895 ) ) ;
#3606 = EDGE_CURVE ( 'NONE', #12662, #13377, #25458, .T. ) ;
#3607 = DIRECTION ( 'NONE',  ( 1.000000000000000000, 0.000000000000000000, -0.000000000000000000 ) ) ;
#3608 = CARTESIAN_POINT ( 'NONE',  ( 30.91344420362547041, 3.401318489841111514, 1.000000000000000000 ) ) ;
#3609 = VERTEX_POINT ( 'NONE', #17872 ) ;
#3610 = CYLINDRICAL_SURFACE ( 'NONE', #18880, 3.000000000000000444 ) ;
#3611 = CARTESIAN_POINT ( 'NONE',  ( 1.999999999999995781, -26.95000000000000284, 5.535898384862237620 ) ) ;
#3613 = EDGE_LOOP ( 'NONE', ( #2635, #3782, #17874, #5164, #7758, #2631, #11486, #4361 ) ) ;
#3612 = CARTESIAN_POINT ( 'NONE',  ( 3.756430356250004987, 25.25312499938548427, 8.999999999999992895 ) ) ;
#3614 = CARTESIAN_POINT ( 'NONE',  ( 3.756430356250002323, 26.56562499938548783, 11.16877607737301403 ) ) ;
#3615 = DIRECTION ( 'NONE',  ( -0.000000000000000000, -0.000000000000000000, -1.000000000000000000 ) ) ;
#3616 = EDGE_LOOP ( 'NONE', ( #1079, #18012, #11226, #20146 ) ) ;
#3617 = CARTESIAN_POINT ( 'NONE',  ( -2.672651547586948120E-15, -29.52812499938548285, 13.33755215474602984 ) ) ;
#3618 = EDGE_LOOP ( 'NONE', ( #580, #15779, #14975, #18678, #23631, #13884, #15664, #1862, #21241 ) ) ;
#3619 = ORIENTED_EDGE ( 'NONE', *, *, #25271, .F. ) ;
#3620 = DIRECTION ( 'NONE',  ( -0.000000000000000000, -0.000000000000000000, 1.000000000000000000 ) ) ;
#3621 = CARTESIAN_POINT ( 'NONE',  ( -3.756430356249996549, 29.52812499938548996, 8.999999999999992895 ) ) ;
#3622 = ADVANCED_FACE ( 'NONE', ( #7678 ), #15662, .T. ) ;
#3623 = CARTESIAN_POINT ( 'NONE',  ( -3.756430356249996994, -8.999999999999992895, 0.8156249993854814972 ) ) ;
#3624 = EDGE_CURVE ( 'NONE', #10717, #21352, #1281, .T. ) ;
#3625 = CARTESIAN_POINT ( 'NONE',  ( -3.756430356249995661, -6.831223922626973533, 4.490624999385484095 ) ) ;
#3626 =( NAMED_UNIT ( * ) SI_UNIT ( $, .STERADIAN. ) SOLID_ANGLE_UNIT ( ) );
#3627 = CARTESIAN_POINT ( 'NONE',  ( 31.10000000000000142, -1.085850696380214537E-13, -6.500000000000000000 ) ) ;
#3628 = CARTESIAN_POINT ( 'NONE',  ( 4.648177544792955347E-16, 28.48750000000000071, 12.99999999999999289 ) ) ;
#3629 = FACE_OUTER_BOUND ( 'NONE', #22399, .T. ) ;
#3630 = CARTESIAN_POINT ( 'NONE',  ( -1.427366165835751044, -29.96717973704832261, 12.74788474329069921 ) ) ;
#3631 = CARTESIAN_POINT ( 'NONE',  ( 0.000000000000000000, 0.000000000000000000, 18.19999999999999929 ) ) ;
#3632 = DIRECTION ( 'NONE',  ( -0.000000000000000000, -0.000000000000000000, 1.000000000000000000 ) ) ;
#3633 = DIRECTION ( 'NONE',  ( 1.000000000000000000, 0.000000000000000000, 0.000000000000000000 ) ) ;
#3634 = ORIENTED_EDGE ( 'NONE', *, *, #18266, .T. ) ;
#3635 = CARTESIAN_POINT ( 'NONE',  ( 1.859271017917182139E-15, 28.93749999999999645, 12.99999999999999289 ) ) ;
#3636 = CARTESIAN_POINT ( 'NONE',  ( -1.878215178124998497, 28.70312499938548356, 12.25316411605951927 ) ) ;
#3638 = EDGE_CURVE ( 'NONE', #22500, #1446, #1699, .T. ) ;
#3637 = DIRECTION ( 'NONE',  ( 0.000000000000000000, 0.000000000000000000, 1.000000000000000000 ) ) ;
#3639 = CARTESIAN_POINT ( 'NONE',  ( 1.071796769724492338, 28.90134618820330203, 12.99999999999999467 ) ) ;
#3640 = ORIENTED_EDGE ( 'NONE', *, *, #7545, .T. ) ;
#3641 = CARTESIAN_POINT ( 'NONE',  ( -3.756430356249996105, 29.49062499938548854, 6.831223922626973533 ) ) ;
#3642 = FACE_OUTER_BOUND ( 'NONE', #24853, .T. ) ;
#3644 = ORIENTED_EDGE ( 'NONE', *, *, #8016, .T. ) ;
#3643 = CARTESIAN_POINT ( 'NONE',  ( 2.000000000000000000, 28.46874999877097423, 12.46410161513774817 ) ) ;
#3645 = ORIENTED_EDGE ( 'NONE', *, *, #19553, .F. ) ;
#3646 = VERTEX_POINT ( 'NONE', #23747 ) ;
#3647 = VERTEX_POINT ( 'NONE', #5836 ) ;
#3648 = ORIENTED_EDGE ( 'NONE', *, *, #466, .T. ) ;
#3649 = CARTESIAN_POINT ( 'NONE',  ( -28.41604871112473418, -11.44867358849319849, -6.500000000000000000 ) ) ;
#3650 = CYLINDRICAL_SURFACE ( 'NONE', #12787, 31.10000000000000142 ) ;
#3651 = DIRECTION ( 'NONE',  ( -0.000000000000000000, -0.000000000000000000, 1.000000000000000000 ) ) ;
#3652 = CARTESIAN_POINT ( 'NONE',  ( 4.006172263299091013E-15, 25.70312499938548356, 4.662447845253954171 ) ) ;
#3653 = CARTESIAN_POINT ( 'NONE',  ( -3.756430356249995661, -6.831223922626973533, 3.928124999385480542 ) ) ;
#3654 = CARTESIAN_POINT ( 'NONE',  ( 4.000000000000003553, -8.999999999999992895, 3.093749998770968457 ) ) ;
#3655 =( NAMED_UNIT ( * ) SI_UNIT ( $, .STERADIAN. ) SOLID_ANGLE_UNIT ( ) );
#3656 = CARTESIAN_POINT ( 'NONE',  ( 3.735045420075836212E-15, 28.96562499938548640, 4.662447845253954171 ) ) ;
#3657 = EDGE_CURVE ( 'NONE', #10871, #19250, #13823, .T. ) ;
#3658 = CARTESIAN_POINT ( 'NONE',  ( -8.831537335106614961E-15, -26.63124999877096855, 12.99999999999999112 ) ) ;
#3659 = DIRECTION ( 'NONE',  ( -0.000000000000000000, 0.000000000000000000, 1.000000000000000000 ) ) ;
#3660 = CARTESIAN_POINT ( 'NONE',  ( -3.999999999999997335, -11.30940107675849404, 1.162499999999998312 ) ) ;
#3661 = CARTESIAN_POINT ( 'NONE',  ( -2.000000000000003997, -25.91874999877096997, 5.535898384862238508 ) ) ;
#3662 = CARTESIAN_POINT ( 'NONE',  ( -3.469446951953614189E-15, -25.00000000000000000, 8.999999999999992895 ) ) ;
#3663 = FACE_OUTER_BOUND ( 'NONE', #758, .T. ) ;
#3664 = CARTESIAN_POINT ( 'NONE',  ( -4.000000000000001776, -25.80624999877096926, 11.30940107675849760 ) ) ;
#3665 = CARTESIAN_POINT ( 'NONE',  ( 3.735045420075836212E-15, 28.06562499938548427, 4.662447845253954171 ) ) ;
#3666 = DIRECTION ( 'NONE',  ( 0.000000000000000000, 0.000000000000000000, 1.000000000000000000 ) ) ;
#3667 = CIRCLE ( 'NONE', #7007, 4.000000000000000000 ) ;
#3668 = DIRECTION ( 'NONE',  ( -0.000000000000000000, -0.000000000000000000, -1.000000000000000000 ) ) ;
#3669 = CYLINDRICAL_SURFACE ( 'NONE', #13071, 31.10000000000000142 ) ;
#3670 = ORIENTED_EDGE ( 'NONE', *, *, #17830, .T. ) ;
#3671 = DIRECTION ( 'NONE',  ( 0.000000000000000000, -0.000000000000000000, 1.000000000000000000 ) ) ;
#3672 = ORIENTED_EDGE ( 'NONE', *, *, #9994, .T. ) ;
#3673 = ORIENTED_EDGE ( 'NONE', *, *, #9968, .T. ) ;
#3674 = CYLINDRICAL_SURFACE ( 'NONE', #355, 0.5000000000000004441 ) ;
#3675 =( BOUNDED_CURVE ( )  B_SPLINE_CURVE ( 2, ( #2416, #8691, #10378, #4260, #8309, #18641, #20600, #4381, #2686 ),
 .UNSPECIFIED., .F., .F. ) 
 B_SPLINE_CURVE_WITH_KNOTS ( ( 3, 2, 2, 2, 3 ),
 ( 0.4750000000000000333, 0.4833333333333333370, 0.5000000000000000000, 0.5166666666666667185, 0.5250000000000000222 ),
 .UNSPECIFIED. ) 
 CURVE ( )  GEOMETRIC_REPRESENTATION_ITEM ( )  RATIONAL_B_SPLINE_CURVE ( ( 0.9330127018922194093, 0.9330127018922196314, 1.000000000000000000, 0.8660254037844387076, 1.000000000000000000, 0.8660254037844387076, 1.000000000000000000, 0.9330127018922194093, 0.9330127018922194093 ) ) 
 REPRESENTATION_ITEM ( '' )  );
#3677 = ORIENTED_EDGE ( 'NONE', *, *, #3960, .T. ) ;
#3676 = AXIS2_PLACEMENT_3D ( 'NONE', #24845, #12547, #399 ) ;
#3678 = CARTESIAN_POINT ( 'NONE',  ( -3.756430356250002323, -27.46562499938548640, 11.16877607737301226 ) ) ;
#3679 = VERTEX_POINT ( 'NONE', #18386 ) ;
#3680 = DIRECTION ( 'NONE',  ( 1.000000000000000000, 0.000000000000000000, 0.000000000000000000 ) ) ;
#3681 = ORIENTED_EDGE ( 'NONE', *, *, #22094, .T. ) ;
#3682 = CARTESIAN_POINT ( 'NONE',  ( 2.620986760973688460E-15, 27.58750000000000213, 13.61880215351699874 ) ) ;
#3683 = CARTESIAN_POINT ( 'NONE',  ( 0.4995657836784091477, 31.50000000000000000, 14.97916666666665897 ) ) ;
#3684 = CIRCLE ( 'NONE', #18312, 0.5000000000000005551 ) ;
#3685 = CARTESIAN_POINT ( 'NONE',  ( 3.756430356250004099, -6.831223922626973533, 0.7406249993854815417 ) ) ;
#3686 = CARTESIAN_POINT ( 'NONE',  ( -4.000000000000000888, 25.71250000000000568, 11.30940107675849404 ) ) ;
#3687 = CARTESIAN_POINT ( 'NONE',  ( 18.64987758779700044, 21.30607496575630222, 12.25316411605951927 ) ) ;
#3688 = CARTESIAN_POINT ( 'NONE',  ( -3.878215178125003604, -29.57031249969274356, 8.999999999999992895 ) ) ;
#3689 = ADVANCED_FACE ( 'NONE', ( #16302 ), #12240, .F. ) ;
#3690 = CIRCLE ( 'NONE', #4117, 31.10000000000000142 ) ;
#3691 = CARTESIAN_POINT ( 'NONE',  ( 2.000000000000000888, 28.97500000000000142, 12.46410161513774817 ) ) ;
#3692 = DIRECTION ( 'NONE',  ( -0.000000000000000000, -1.000000000000000000, -0.000000000000000000 ) ) ;
#3693 = EDGE_CURVE ( 'NONE', #2271, #408, #181, .T. ) ;
#3694 = CARTESIAN_POINT ( 'NONE',  ( 23.40315227927642283, 18.09075752335759901, 6.831223922626973533 ) ) ;
#3695 = CARTESIAN_POINT ( 'NONE',  ( -24.86329371854788661, -18.68225429291705098, 1.000000000000000000 ) ) ;
#3696 = ORIENTED_EDGE ( 'NONE', *, *, #14089, .F. ) ;
#3698 = EDGE_CURVE ( 'NONE', #17369, #9796, #12489, .T. ) ;
#3697 = ORIENTED_EDGE ( 'NONE', *, *, #5014, .T. ) ;
#3699 = CARTESIAN_POINT ( 'NONE',  ( -3.999999999999998224, 29.66874999877097352, 8.999999999999992895 ) ) ;
#3700 = ORIENTED_EDGE ( 'NONE', *, *, #1391, .T. ) ;
#3701 = CARTESIAN_POINT ( 'NONE',  ( -22.32573188046889356, 21.65113613650366986, -2.750000000000000000 ) ) ;
#3702 = AXIS2_PLACEMENT_3D ( 'NONE', #22447, #10666, #24808 ) ;
#3703 = CARTESIAN_POINT ( 'NONE',  ( -3.999999999999999112, 29.31250000000000000, 11.30940107675849404 ) ) ;
#3704 = DIRECTION ( 'NONE',  ( 1.000000000000000000, 0.000000000000000000, 0.000000000000000000 ) ) ;
#3705 = EDGE_CURVE ( 'NONE', #10879, #24971, #8191, .T. ) ;
#3706 = ORIENTED_EDGE ( 'NONE', *, *, #670, .F. ) ;
#3707 = ORIENTED_EDGE ( 'NONE', *, *, #13635, .T. ) ;
#3708 = AXIS2_PLACEMENT_3D ( 'NONE', #15844, #23817, #4545 ) ;
#3709 = ORIENTED_EDGE ( 'NONE', *, *, #13815, .T. ) ;
#3710 = CARTESIAN_POINT ( 'NONE',  ( -3.469446951953614189E-15, -30.00000000000000355, 4.999999999999992006 ) ) ;
#3711 = FACE_OUTER_BOUND ( 'NONE', #15993, .T. ) ;
#3712 = CARTESIAN_POINT ( 'NONE',  ( 1.878215178124998275, 26.86562499938548854, 12.25316411605952283 ) ) ;
#3713 = DIRECTION ( 'NONE',  ( 0.000000000000000000, 1.000000000000000000, 0.000000000000000000 ) ) ;
#3714 = CARTESIAN_POINT ( 'NONE',  ( 2.000000000000005329, 26.42500000000000426, 5.535898384862238508 ) ) ;
#3715 =( BOUNDED_SURFACE ( )  B_SPLINE_SURFACE ( 1, 2, ( 
 ( #17727, #8049, #23994, #4244, #23866, #13665, #25698, #12223, #203, #16030, #20190, #7779, #10246, #5951, #17988, #21636, #17850, #20058, #22024, #15759, #23724, #4106, #1906, #12084, #9991, #23606, #5812, #3861, #25821, #11834, #76, #2163, #19804, #9868, #7905, #18241, #13937, #21904, #24114, #3985, #11952, #323, #19922, #2023, #6197, #15641, #14453, #4372, #16664, #22413, #14570, #465, #24250, #12865, #22690, #22814, #24506, #22553, #6587, #22296, #20314, #14331, #2932, #4494, #18510, #20445, #6857, #8820, #20843, #12350, #10893, #24632, #18630, #2795, #2407, #18893, #8435, #10365, #8295, #12469, #14840, #10510, #4773, #24389, #2677, #6467, #10637, #715, #596, #16282, #8681, #16547, #4633, #6337, #18366, #12613, #2542, #8563, #6720, #16422, #20589, #12745, #4889, #14711, #20716, #10761, #16810, #18749, #839, #24774, #19012, #16933, #1095, #25405, #3307, #25166, #5024, #25024, #1223, #7247, #5542 ),
 ( #7491, #13005, #24902, #13254, #11283, #3065, #19264, #9340, #15483, #9204, #6980, #11033, #23452, #21369, #1366, #13525, #9070, #21495, #17194, #17324, #14961, #3183, #5403, #25287, #17055, #7115, #7368, #13140, #15345, #21225, #8959, #20986, #22937, #11150, #15101, #23315, #13390, #23076, #21105, #5160, #3572, #19131, #15227, #3447, #23193, #5278, #11544, #11421, #19395, #1487, #978, #9459, #17438, #1996, #25674, #25794, #11671, #9583, #24089, #8018, #8148, #9843, #7877, #17825, #7630, #5663, #25546, #14160, #7754, #3831, #5783, #18099, #20031, #6172, #15615, #22128, #9967, #3963, #14034, #23582, #4216, #19648, #13643, #19510, #15738, #177, #21748, #16003, #17958, #21611, #4078, #2135, #16127, #45, #17706, #17570, #23970, #5923, #11928, #6051, #1754, #22001, #12051, #1610, #10099, #23700, #3691, #9724, #13769, #11810, #19784, #1881, #15865, #23834, #13909, #21879, #19897, #10733, #8270, #24221, #18606 ) ),
 .UNSPECIFIED., .F., .F., .T. ) 
 B_SPLINE_SURFACE_WITH_KNOTS ( ( 2, 2 ),
 ( 3, 2, 2, 2, 2, 2, 2, 2, 2, 2, 2, 2, 2, 2, 2, 2, 2, 2, 2, 2, 2, 2, 2, 2, 2, 2, 2, 2, 2, 2, 2, 2, 2, 2, 2, 2, 2, 2, 2, 2, 2, 2, 2, 2, 2, 2, 2, 2, 2, 2, 2, 2, 2, 2, 2, 2, 2, 2, 2, 2, 3 ),
 ( 0.000000000000000000, 1.000000000000000000 ),
 ( 0.000000000000000000, 0.01666666666666666644, 0.03333333333333333287, 0.05000000000000000278, 0.06666666666666666574, 0.08333333333333332871, 0.1000000000000000056, 0.1166666666666666685, 0.1333333333333333315, 0.1499999999999999944, 0.1666666666666666574, 0.1833333333333333204, 0.2000000000000000111, 0.2166666666666666741, 0.2333333333333333370, 0.2500000000000000000, 0.2666666666666666630, 0.2833333333333333259, 0.2999999999999999889, 0.3166666666666666519, 0.3333333333333333148, 0.3499999999999999778, 0.3666666666666666408, 0.3833333333333333592, 0.4000000000000000222, 0.4166666666666666852, 0.4333333333333333481, 0.4500000000000000111, 0.4666666666666666741, 0.4833333333333333370, 0.5000000000000000000, 0.5166666666666667185, 0.5333333333333333259, 0.5500000000000000444, 0.5666666666666666519, 0.5833333333333333703, 0.5999999999999999778, 0.6166666666666666963, 0.6333333333333333037, 0.6500000000000000222, 0.6666666666666666297, 0.6833333333333333481, 0.6999999999999999556, 0.7166666666666666741, 0.7333333333333332815, 0.7500000000000000000, 0.7666666666666667185, 0.7833333333333333259, 0.8000000000000000444, 0.8166666666666666519, 0.8333333333333333703, 0.8499999999999999778, 0.8666666666666666963, 0.8833333333333333037, 0.9000000000000000222, 0.9166666666666666297, 0.9333333333333333481, 0.9499999999999999556, 0.9666666666666666741, 0.9833333333333332815, 1.000000000000000000 ),
 .UNSPECIFIED. ) 
 GEOMETRIC_REPRESENTATION_ITEM ( )  RATIONAL_B_SPLINE_SURFACE ( (
 ( 1.000000000000000000, 0.8660254037844387076, 1.000000000000000000, 0.8660254037844387076, 1.000000000000000000, 0.8660254037844387076, 1.000000000000000000, 0.8660254037844387076, 1.000000000000000000, 0.8660254037844387076, 1.000000000000000000, 0.8660254037844387076, 1.000000000000000000, 0.8660254037844387076, 1.000000000000000000, 0.8660254037844387076, 1.000000000000000000, 0.8660254037844387076, 1.000000000000000000, 0.8660254037844387076, 1.000000000000000000, 0.8660254037844387076, 1.000000000000000000, 0.8660254037844387076, 1.000000000000000000, 0.8660254037844387076, 1.000000000000000000, 0.8660254037844387076, 1.000000000000000000, 0.8660254037844387076, 1.000000000000000000, 0.8660254037844387076, 1.000000000000000000, 0.8660254037844387076, 1.000000000000000000, 0.8660254037844387076, 1.000000000000000000, 0.8660254037844387076, 1.000000000000000000, 0.8660254037844387076, 1.000000000000000000, 0.8660254037844387076, 1.000000000000000000, 0.8660254037844387076, 1.000000000000000000, 0.8660254037844387076, 1.000000000000000000, 0.8660254037844387076, 1.000000000000000000, 0.8660254037844387076, 1.000000000000000000, 0.8660254037844387076, 1.000000000000000000, 0.8660254037844387076, 1.000000000000000000, 0.8660254037844387076, 1.000000000000000000, 0.8660254037844387076, 1.000000000000000000, 0.8660254037844387076, 1.000000000000000000, 0.8660254037844387076, 1.000000000000000000, 0.8660254037844387076, 1.000000000000000000, 0.8660254037844387076, 1.000000000000000000, 0.8660254037844387076, 1.000000000000000000, 0.8660254037844387076, 1.000000000000000000, 0.8660254037844387076, 1.000000000000000000, 0.8660254037844387076, 1.000000000000000000, 0.8660254037844387076, 1.000000000000000000, 0.8660254037844387076, 1.000000000000000000, 0.8660254037844387076, 1.000000000000000000, 0.8660254037844387076, 1.000000000000000000, 0.8660254037844387076, 1.000000000000000000, 0.8660254037844387076, 1.000000000000000000, 0.8660254037844387076, 1.000000000000000000, 0.8660254037844387076, 1.000000000000000000, 0.8660254037844387076, 1.000000000000000000, 0.8660254037844387076, 1.000000000000000000, 0.8660254037844387076, 1.000000000000000000, 0.8660254037844387076, 1.000000000000000000, 0.8660254037844387076, 1.000000000000000000, 0.8660254037844387076, 1.000000000000000000, 0.8660254037844387076, 1.000000000000000000, 0.8660254037844387076, 1.000000000000000000, 0.8660254037844387076, 1.000000000000000000, 0.8660254037844387076, 1.000000000000000000, 0.8660254037844387076, 1.000000000000000000, 0.8660254037844387076, 1.000000000000000000, 0.8660254037844387076, 1.000000000000000000, 0.8660254037844387076, 1.000000000000000000, 0.8660254037844387076, 1.000000000000000000),
 ( 1.000000000000000000, 0.8660254037844387076, 1.000000000000000000, 0.8660254037844387076, 1.000000000000000000, 0.8660254037844387076, 1.000000000000000000, 0.8660254037844387076, 1.000000000000000000, 0.8660254037844387076, 1.000000000000000000, 0.8660254037844387076, 1.000000000000000000, 0.8660254037844387076, 1.000000000000000000, 0.8660254037844387076, 1.000000000000000000, 0.8660254037844387076, 1.000000000000000000, 0.8660254037844387076, 1.000000000000000000, 0.8660254037844387076, 1.000000000000000000, 0.8660254037844387076, 1.000000000000000000, 0.8660254037844387076, 1.000000000000000000, 0.8660254037844387076, 1.000000000000000000, 0.8660254037844387076, 1.000000000000000000, 0.8660254037844387076, 1.000000000000000000, 0.8660254037844387076, 1.000000000000000000, 0.8660254037844387076, 1.000000000000000000, 0.8660254037844387076, 1.000000000000000000, 0.8660254037844387076, 1.000000000000000000, 0.8660254037844387076, 1.000000000000000000, 0.8660254037844387076, 1.000000000000000000, 0.8660254037844387076, 1.000000000000000000, 0.8660254037844387076, 1.000000000000000000, 0.8660254037844387076, 1.000000000000000000, 0.8660254037844387076, 1.000000000000000000, 0.8660254037844387076, 1.000000000000000000, 0.8660254037844387076, 1.000000000000000000, 0.8660254037844387076, 1.000000000000000000, 0.8660254037844387076, 1.000000000000000000, 0.8660254037844387076, 1.000000000000000000, 0.8660254037844387076, 1.000000000000000000, 0.8660254037844387076, 1.000000000000000000, 0.8660254037844387076, 1.000000000000000000, 0.8660254037844387076, 1.000000000000000000, 0.8660254037844387076, 1.000000000000000000, 0.8660254037844387076, 1.000000000000000000, 0.8660254037844387076, 1.000000000000000000, 0.8660254037844387076, 1.000000000000000000, 0.8660254037844387076, 1.000000000000000000, 0.8660254037844387076, 1.000000000000000000, 0.8660254037844387076, 1.000000000000000000, 0.8660254037844387076, 1.000000000000000000, 0.8660254037844387076, 1.000000000000000000, 0.8660254037844387076, 1.000000000000000000, 0.8660254037844387076, 1.000000000000000000, 0.8660254037844387076, 1.000000000000000000, 0.8660254037844387076, 1.000000000000000000, 0.8660254037844387076, 1.000000000000000000, 0.8660254037844387076, 1.000000000000000000, 0.8660254037844387076, 1.000000000000000000, 0.8660254037844387076, 1.000000000000000000, 0.8660254037844387076, 1.000000000000000000, 0.8660254037844387076, 1.000000000000000000, 0.8660254037844387076, 1.000000000000000000, 0.8660254037844387076, 1.000000000000000000, 0.8660254037844387076, 1.000000000000000000, 0.8660254037844387076, 1.000000000000000000, 0.8660254037844387076, 1.000000000000000000, 0.8660254037844387076, 1.000000000000000000) ) ) 
 REPRESENTATION_ITEM ( '' )  SURFACE ( )  );
#3716 = AXIS2_PLACEMENT_3D ( 'NONE', #17008, #23151, #11229 ) ;
#3717 = CYLINDRICAL_SURFACE ( 'NONE', #12602, 4.000000000000000000 ) ;
#3718 = CIRCLE ( 'NONE', #7076, 31.10000000000000142 ) ;
#3719 = CYLINDRICAL_SURFACE ( 'NONE', #13861, 31.10000000000000142 ) ;
#3720 = EDGE_CURVE ( 'NONE', #21859, #24971, #11056, .T. ) ;
#3721 = VECTOR ( 'NONE', #985, 1000.000000000000000 ) ;
#3722 = PRODUCT_DEFINITION ( 'UNKNOWN', '', #21072, #20916 ) ;
#3723 = CARTESIAN_POINT ( 'NONE',  ( 5.112995299272250684E-15, 26.40624999877096712, 4.999999999999992006 ) ) ;
#3724 = CARTESIAN_POINT ( 'NONE',  ( 22.38876845931909187, 16.73191420982663757, 11.30940107675849760 ) ) ;
#3725 = CARTESIAN_POINT ( 'NONE',  ( 23.05843772344798381, 17.74604296752915999, 8.999999999999992895 ) ) ;
#3726 = DIRECTION ( 'NONE',  ( 0.000000000000000000, 0.000000000000000000, 1.000000000000000000 ) ) ;
#3727 = CARTESIAN_POINT ( 'NONE',  ( -3.756430356249996994, 29.41562499938548569, 8.999999999999992895 ) ) ;
#3728 = CARTESIAN_POINT ( 'NONE',  ( 4.000000000000001776, 27.19374999877097210, 8.999999999999992895 ) ) ;
#3729 = CARTESIAN_POINT ( 'NONE',  ( 23.00540471485899019, 17.69300995894016992, 6.831223922626973533 ) ) ;
#3730 = AXIS2_PLACEMENT_3D ( 'NONE', #6727, #9441, #1591 ) ;
#3731 = CARTESIAN_POINT ( 'NONE',  ( 18.03564233677035489, 18.03564233677029094, 4.999999999999992006 ) ) ;
#3732 = VERTEX_POINT ( 'NONE', #2309 ) ;
#3733 = CARTESIAN_POINT ( 'NONE',  ( 4.000000000000003553, 26.33124999877097139, 6.690598923241489970 ) ) ;
#3734 = CARTESIAN_POINT ( 'NONE',  ( -4.000000000000003553, -26.38750000000000284, 6.690598923241489970 ) ) ;
#3735 = EDGE_CURVE ( 'NONE', #2553, #19625, #4268, .T. ) ;
#3737 = ORIENTED_EDGE ( 'NONE', *, *, #25399, .T. ) ;
#3736 = DIRECTION ( 'NONE',  ( -0.9659258262890673130, 0.2588190451025242922, 0.000000000000000000 ) ) ;
#3738 = CARTESIAN_POINT ( 'NONE',  ( 2.672651547586948120E-15, 29.19062499938548427, 13.33755215474603162 ) ) ;
#3739 = AXIS2_PLACEMENT_3D ( 'NONE', #11567, #19535, #19038 ) ;
#3740 = EDGE_CURVE ( 'NONE', #1683, #14407, #10452, .T. ) ;
#3741 = CARTESIAN_POINT ( 'NONE',  ( -7.234255490826573265, 30.12293631110053838, 1.000000000000000000 ) ) ;
#3742 = AXIS2_PLACEMENT_3D ( 'NONE', #24689, #7293, #18939 ) ;
#3743 = ORIENTED_EDGE ( 'NONE', *, *, #22970, .T. ) ;
#3744 = CARTESIAN_POINT ( 'NONE',  ( 1.859271017917182139E-15, 26.18124999877096570, 12.99999999999999289 ) ) ;
#3745 = ORIENTED_EDGE ( 'NONE', *, *, #16115, .T. ) ;
#3746 = EDGE_LOOP ( 'NONE', ( #10352, #14248, #7120, #2218 ) ) ;
#3747 = PRESENTATION_STYLE_ASSIGNMENT (( #21662 ) ) ;
#3748 = CARTESIAN_POINT ( 'NONE',  ( 3.756430356250003211, 29.30312499938548498, 8.999999999999992895 ) ) ;
#3749 = AXIS2_PLACEMENT_3D ( 'NONE', #7003, #19036, #17081 ) ;
#3750 = AXIS2_PLACEMENT_3D ( 'NONE', #25658, #11913, #23434 ) ;
#3751 = APPLICATION_CONTEXT ( 'automotive_design' ) ;
#3752 = CARTESIAN_POINT ( 'NONE',  ( 2.672651547586948120E-15, -13.33755215474603162, 3.178124999385480987 ) ) ;
#3753 = AXIS2_PLACEMENT_3D ( 'NONE', #25107, #5483, #24973 ) ;
#3754 = LINE ( 'NONE', #23759, #24633 ) ;
#3755 = DIRECTION ( 'NONE',  ( 0.000000000000000000, 1.000000000000000000, 0.000000000000000000 ) ) ;
#3756 = AXIS2_PLACEMENT_3D ( 'NONE', #12719, #13228, #12971 ) ;
#3757 = AXIS2_PLACEMENT_3D ( 'NONE', #8601, #22066, #24542 ) ;
#3758 = CYLINDRICAL_SURFACE ( 'NONE', #13434, 4.000000000000000000 ) ;
#3759 = CYLINDRICAL_SURFACE ( 'NONE', #23855, 4.000000000000000000 ) ;
#3760 = DIRECTION ( 'NONE',  ( 1.000000000000000000, 0.000000000000000000, 0.000000000000000000 ) ) ;
#3761 = CARTESIAN_POINT ( 'NONE',  ( 2.000000000000000888, 25.76874999877096784, 12.46410161513774817 ) ) ;
#3762 = CARTESIAN_POINT ( 'NONE',  ( -23.01025686871616216, 20.92219106202074741, -6.500000000000000000 ) ) ;
#3763 = CARTESIAN_POINT ( 'NONE',  ( 15.94967733227004558, 21.60653158176235777, 11.30940107675849404 ) ) ;
#3764 = ORIENTED_EDGE ( 'NONE', *, *, #24587, .T. ) ;
#3765 = DIRECTION ( 'NONE',  ( 0.000000000000000000, 0.000000000000000000, 1.000000000000000000 ) ) ;
#3766 = CARTESIAN_POINT ( 'NONE',  ( -1.878215178125000939, -28.32812499938548711, 12.25316411605952283 ) ) ;
#3767 = CARTESIAN_POINT ( 'NONE',  ( -3.756430356249995661, 26.79062499938548925, 6.831223922626973533 ) ) ;
#3768 = VECTOR ( 'NONE', #19158, 1000.000000000000000 ) ;
#3769 = DIRECTION ( 'NONE',  ( 0.4817536741017267032, 0.8763066800438573667, 0.000000000000000000 ) ) ;
#3770 = CARTESIAN_POINT ( 'NONE',  ( 5.335677986744788548, 30.63887302793246548, -6.500000000000000000 ) ) ;
#3771 = ADVANCED_FACE ( 'NONE', ( #20035 ), #2138, .T. ) ;
#3772 = DIRECTION ( 'NONE',  ( 1.000000000000000000, 0.000000000000000000, 0.000000000000000000 ) ) ;
#3773 = EDGE_LOOP ( 'NONE', ( #1414, #13122, #6814, #9882 ) ) ;
#3774 = CARTESIAN_POINT ( 'NONE',  ( 2.000000000000000888, -12.46410161513774817, 2.624999999999998668 ) ) ;
#3775 = FACE_OUTER_BOUND ( 'NONE', #22218, .T. ) ;
#3777 = EDGE_LOOP ( 'NONE', ( #22597, #13485, #22888, #23715 ) ) ;
#3776 = CARTESIAN_POINT ( 'NONE',  ( 3.999999999999995559, -26.48124999877096641, 6.690598923241487306 ) ) ;
#3778 = EDGE_CURVE ( 'NONE', #7533, #9331, #15068, .T. ) ;
#3779 = ORIENTED_EDGE ( 'NONE', *, *, #17901, .T. ) ;
#3780 = AXIS2_PLACEMENT_3D ( 'NONE', #4080, #1882, #9844 ) ;
#3781 = VERTEX_POINT ( 'NONE', #4220 ) ;
#3782 = ORIENTED_EDGE ( 'NONE', *, *, #12659, .T. ) ;
#3783 = VERTEX_POINT ( 'NONE', #1997 ) ;
#3784 = DIRECTION ( 'NONE',  ( 0.9822872507286911636, 0.1873813145857119722, 0.000000000000000000 ) ) ;
#3785 = CIRCLE ( 'NONE', #17165, 0.5000000000000004441 ) ;
#3786 = CARTESIAN_POINT ( 'NONE',  ( -3.574812588380618106, 38.86762122992235646, 13.35267830710396630 ) ) ;
#3787 = CIRCLE ( 'NONE', #2536, 5.500000000000000000 ) ;
#3788 = SURFACE_STYLE_FILL_AREA ( #22223 ) ;
#3789 = LINE ( 'NONE', #9159, #13919 ) ;
#3790 = CIRCLE ( 'NONE', #882, 6.000000000000000000 ) ;
#3791 = CARTESIAN_POINT ( 'NONE',  ( 2.672651547586948120E-15, -13.33755215474602984, 2.278124999385481519 ) ) ;
#3792 = CARTESIAN_POINT ( 'NONE',  ( -3.999999999999997335, -11.30940107675849404, 4.706249998770967835 ) ) ;
#3793 = CARTESIAN_POINT ( 'NONE',  ( -3.756430356249997882, 29.11562499938548143, 11.16877607737301226 ) ) ;
#3794 = CYLINDRICAL_SURFACE ( 'NONE', #9205, 31.10000000000000142 ) ;
#3795 = CARTESIAN_POINT ( 'NONE',  ( -17.08421000182742233, 25.98730014090460472, 1.000000000000000000 ) ) ;
#3796 = ADVANCED_BREP_SHAPE_REPRESENTATION ( '', ( #22081, #21036 ), #9344 ) ;
#3797 = CARTESIAN_POINT ( 'NONE',  ( 4.000000000000003553, -8.999999999999992895, 2.249999999999998668 ) ) ;
#3798 = CARTESIAN_POINT ( 'NONE',  ( -24.66042852506064165, 18.28012134629622309, -6.500000000000000000 ) ) ;
#3799 = CARTESIAN_POINT ( 'NONE',  ( 3.999999999999970690, -11.30940107675851536, 2.606249998770964194 ) ) ;
#3800 = DIRECTION ( 'NONE',  ( 0.000000000000000000, 0.000000000000000000, 1.000000000000000000 ) ) ;
#3801 = CARTESIAN_POINT ( 'NONE',  ( -3.752267015613588906E-15, -26.40624999877097068, 4.381197846482986158 ) ) ;
#3802 = VECTOR ( 'NONE', #23048, 1000.000000000000000 ) ;
#3803 = CARTESIAN_POINT ( 'NONE',  ( 2.672651547586948120E-15, 29.19062499938548783, 13.33755215474602984 ) ) ;
#3804 = AXIS2_PLACEMENT_3D ( 'NONE', #21167, #5095, #3125 ) ;
#3805 = PLANE ( 'NONE',  #19525 ) ;
#3806 = CARTESIAN_POINT ( 'NONE',  ( -13.24173596767398742, -28.14012133169310559, -6.500000000000000000 ) ) ;
#3807 = DIRECTION ( 'NONE',  ( 0.000000000000000000, 0.000000000000000000, -1.000000000000000000 ) ) ;
#3808 = EDGE_LOOP ( 'NONE', ( #6930, #25612, #13410, #11872 ) ) ;
#3809 = DIRECTION ( 'NONE',  ( 0.000000000000000000, 0.000000000000000000, -1.000000000000000000 ) ) ;
#3810 = ORIENTED_EDGE ( 'NONE', *, *, #19844, .T. ) ;
#3811 = EDGE_CURVE ( 'NONE', #9446, #9323, #7124, .T. ) ;
#3812 = ORIENTED_EDGE ( 'NONE', *, *, #17316, .F. ) ;
#3813 = CARTESIAN_POINT ( 'NONE',  ( -27.00874656207282953, 15.41874213889444079, -2.750000000000000000 ) ) ;
#3814 = ORIENTED_EDGE ( 'NONE', *, *, #4652, .T. ) ;
#3815 = CARTESIAN_POINT ( 'NONE',  ( 1.878215178124998497, -28.70312499938548356, 12.25316411605951927 ) ) ;
#3816 = ORIENTED_EDGE ( 'NONE', *, *, #6574, .T. ) ;
#3817 = CARTESIAN_POINT ( 'NONE',  ( 26.25859848311259981, -16.66421332384692278, -6.500000000000000000 ) ) ;
#3818 = EDGE_CURVE ( 'NONE', #12311, #364, #25087, .T. ) ;
#3819 = ORIENTED_EDGE ( 'NONE', *, *, #11622, .F. ) ;
#3820 = CARTESIAN_POINT ( 'NONE',  ( -3.999999999999996447, 27.02500000000000213, 8.999999999999992895 ) ) ;
#3821 = CYLINDRICAL_SURFACE ( 'NONE', #14763, 31.10000000000000142 ) ;
#3822 = AXIS2_PLACEMENT_3D ( 'NONE', #22267, #20290, #22386 ) ;
#3823 = ADVANCED_FACE ( 'NONE', ( #5665 ), #16130, .T. ) ;
#3824 = CARTESIAN_POINT ( 'NONE',  ( 0.000000000000000000, 0.000000000000000000, -6.500000000000000000 ) ) ;
#3825 = LINE ( 'NONE', #5917, #14627 ) ;
#3826 = CARTESIAN_POINT ( 'NONE',  ( 22.10157009459123856, 19.44537271663178757, 5.746835883940462963 ) ) ;
#3827 = CIRCLE ( 'NONE', #7604, 0.5000000000000006661 ) ;
#3828 = CARTESIAN_POINT ( 'NONE',  ( -3.999999999999996447, 27.38124999877097210, 6.690598923241487306 ) ) ;
#3829 = DIRECTION ( 'NONE',  ( 0.000000000000000000, 0.000000000000000000, -1.000000000000000000 ) ) ;
#3830 = APPLICATION_PROTOCOL_DEFINITION ( 'draft international standard', 'automotive_design', 1998, #2921 ) ;
#3831 = CARTESIAN_POINT ( 'NONE',  ( 2.620986760973688460E-15, 27.58750000000000213, 13.61880215351699874 ) ) ;
#3832 = CARTESIAN_POINT ( 'NONE',  ( 2.672651547586948120E-15, -13.33755215474603162, 0.5906249993854857383 ) ) ;
#3833 = CARTESIAN_POINT ( 'NONE',  ( 20.00449278107117834, 20.00449278107111439, 13.33755215474603162 ) ) ;
#3834 = LINE ( 'NONE', #11814, #3235 ) ;
#3835 = AXIS2_PLACEMENT_3D ( 'NONE', #10057, #4173, #6880 ) ;
#3836 = ORIENTED_EDGE ( 'NONE', *, *, #841, .F. ) ;
#3837 = ORIENTED_EDGE ( 'NONE', *, *, #7363, .F. ) ;
#3838 = CARTESIAN_POINT ( 'NONE',  ( -2.003086131649545506E-15, 26.04062499938549280, 13.33755215474602984 ) ) ;
#3839 = AXIS2_PLACEMENT_3D ( 'NONE', #11898, #24057, #1850 ) ;
#3840 = VECTOR ( 'NONE', #9694, 999.9999999999998863 ) ;
#3841 = EDGE_LOOP ( 'NONE', ( #22776, #15990, #22244, #20178 ) ) ;
#3842 = CARTESIAN_POINT ( 'NONE',  ( -3.137519842735244810E-15, 26.46249999999999858, 4.999999999999991118 ) ) ;
#3843 = CARTESIAN_POINT ( 'NONE',  ( -3.756430356249995661, 29.49062499938548498, 6.831223922626973533 ) ) ;
#3844 = CARTESIAN_POINT ( 'NONE',  ( -5.827558883615604479, 30.54913349766230724, -6.500000000000000000 ) ) ;
#3845 = ORIENTED_EDGE ( 'NONE', *, *, #16029, .F. ) ;
#3846 = ORIENTED_EDGE ( 'NONE', *, *, #6041, .F. ) ;
#3847 = VECTOR ( 'NONE', #2018, 1000.000000000000000 ) ;
#3848 = EDGE_CURVE ( 'NONE', #10226, #10048, #18220, .T. ) ;
#3849 = CARTESIAN_POINT ( 'NONE',  ( 3.752267015613588906E-15, -4.381197846482986158, 4.162500000000000533 ) ) ;
#3850 = ORIENTED_EDGE ( 'NONE', *, *, #19484, .F. ) ;
#3851 = DIRECTION ( 'NONE',  ( -0.000000000000000000, -0.000000000000000000, -1.000000000000000000 ) ) ;
#3852 = CARTESIAN_POINT ( 'NONE',  ( -28.72825533807115050, 11.91206721063083229, -2.750000000000000000 ) ) ;
#3853 = CARTESIAN_POINT ( 'NONE',  ( 3.756430356250003211, 28.29062499938548569, 8.999999999999992895 ) ) ;
#3854 = ADVANCED_FACE ( 'NONE', ( #18101 ), #8019, .T. ) ;
#3855 = EDGE_CURVE ( 'NONE', #14526, #1168, #12890, .T. ) ;
#3856 = CARTESIAN_POINT ( 'NONE',  ( -3.959305671612554781E-15, -30.00000000000000355, 12.99999999999999289 ) ) ;
#3857 = CARTESIAN_POINT ( 'NONE',  ( 2.000000000000000000, 26.72500000000000497, 12.46410161513774817 ) ) ;
#3858 = CIRCLE ( 'NONE', #15131, 0.5000000000000000000 ) ;
#3859 = AXIS2_PLACEMENT_3D ( 'NONE', #471, #14196, #24256 ) ;
#3860 = EDGE_CURVE ( 'NONE', #23657, #4330, #17268, .T. ) ;
#3861 = CARTESIAN_POINT ( 'NONE',  ( 3.735045420075836212E-15, 26.15312499938548285, 4.662447845253954171 ) ) ;
#3862 = PRESENTATION_STYLE_ASSIGNMENT (( #9747 ) ) ;
#3863 = CARTESIAN_POINT ( 'NONE',  ( 1.999999999999998224, -28.84374999877096712, 12.46410161513774639 ) ) ;
#3864 = CARTESIAN_POINT ( 'NONE',  ( -0.7500000000000001110, 0.000000000000000000, 15.00000000000000178 ) ) ;
#3865 = CARTESIAN_POINT ( 'NONE',  ( 16.94404624418269023, 22.60090049367499532, 11.30940107675849404 ) ) ;
#3866 = CARTESIAN_POINT ( 'NONE',  ( 21.46517399152334704, 18.80897661356389605, 5.746835883940462963 ) ) ;
#3867 = FACE_OUTER_BOUND ( 'NONE', #9675, .T. ) ;
#3868 = FACE_OUTER_BOUND ( 'NONE', #8136, .T. ) ;
#3869 = CARTESIAN_POINT ( 'NONE',  ( 4.000000000000063061, -11.30940107675846207, 3.056249998770965259 ) ) ;
#3870 =( GEOMETRIC_REPRESENTATION_CONTEXT ( 3 ) GLOBAL_UNCERTAINTY_ASSIGNED_CONTEXT ( ( #14901 ) ) GLOBAL_UNIT_ASSIGNED_CONTEXT ( ( #12798, #14386, #4551 ) ) REPRESENTATION_CONTEXT ( 'NONE', 'WORKASPACE' ) );
#3871 = FACE_OUTER_BOUND ( 'NONE', #10260, .T. ) ;
#3872 = CARTESIAN_POINT ( 'NONE',  ( 20.81103645292755289, 15.15418220343510392, 6.690598923241489970 ) ) ;
#3873 = ORIENTED_EDGE ( 'NONE', *, *, #7691, .F. ) ;
#3874 = CARTESIAN_POINT ( 'NONE',  ( -3.999999999999996003, 26.93124999877096926, 6.690598923241487306 ) ) ;
#3875 = EDGE_CURVE ( 'NONE', #6033, #18161, #25068, .T. ) ;
#3876 = CARTESIAN_POINT ( 'NONE',  ( -2.620986760973688460E-15, -25.78750000000000142, 13.61880215351699874 ) ) ;
#3878 = ORIENTED_EDGE ( 'NONE', *, *, #9853, .F. ) ;
#3877 = CARTESIAN_POINT ( 'NONE',  ( 26.49999999999999645, 0.5000000000000000000, 19.00000000000000000 ) ) ;
#3879 = CARTESIAN_POINT ( 'NONE',  ( -3.756430356249996994, 29.52812499938548640, 8.999999999999992895 ) ) ;
#3880 = CARTESIAN_POINT ( 'NONE',  ( 3.999999999999995559, -29.63124999877096855, 6.690598923241487306 ) ) ;
#3881 = VERTEX_POINT ( 'NONE', #5512 ) ;
#3882 = DIRECTION ( 'NONE',  ( 1.000000000000000000, 0.000000000000000000, 0.000000000000000000 ) ) ;
#3883 = ORIENTED_EDGE ( 'NONE', *, *, #1634, .F. ) ;
#3884 = ORIENTED_EDGE ( 'NONE', *, *, #19484, .T. ) ;
#3885 = CARTESIAN_POINT ( 'NONE',  ( 1.878215178125001605, 26.41562499938548925, 12.25316411605952283 ) ) ;
#3886 =( BOUNDED_CURVE ( )  B_SPLINE_CURVE ( 2, ( #18085, #14023, #19886, #1986, #1869 ),
 .UNSPECIFIED., .F., .F. ) 
 B_SPLINE_CURVE_WITH_KNOTS ( ( 3, 2, 3 ),
 ( 0.000000000000000000, 0.01666666666666666644, 0.02500000000000000486 ),
 .UNSPECIFIED. ) 
 CURVE ( )  GEOMETRIC_REPRESENTATION_ITEM ( )  RATIONAL_B_SPLINE_CURVE ( ( 1.000000000000000000, 0.8660254037844387076, 1.000000000000000000, 0.9330127018922194093, 0.9330127018922194093 ) ) 
 REPRESENTATION_ITEM ( '' )  );
#3887 = ADVANCED_FACE ( 'NONE', ( #13232 ), #3161, .T. ) ;
#3888 = AXIS2_PLACEMENT_3D ( 'NONE', #9542, #15191, #15698 ) ;
#3889 = CARTESIAN_POINT ( 'NONE',  ( -1.878215178124995832, -5.746835883940462963, 2.990624999385481431 ) ) ;
#3890 = EDGE_CURVE ( 'NONE', #4940, #20266, #4620, .T. ) ;
#3891 = DIRECTION ( 'NONE',  ( 1.000000000000000000, 0.000000000000000000, 0.000000000000000000 ) ) ;
#3892 =( LENGTH_UNIT ( ) NAMED_UNIT ( * ) SI_UNIT ( .MILLI., .METRE. ) );
#3893 = EDGE_CURVE ( 'NONE', #12074, #337, #1209, .T. ) ;
#3894 = CARTESIAN_POINT ( 'NONE',  ( -30.24338421796790044, -7.248980000273874680, -6.500000000000000000 ) ) ;
#3895 = CARTESIAN_POINT ( 'NONE',  ( -29.57785765677917311, 9.610428525061202265, 1.000000000000000000 ) ) ;
#3896 = CARTESIAN_POINT ( 'NONE',  ( -8.366719580627318441E-15, 29.55624999877097281, 4.999999999999992006 ) ) ;
#3897 = CARTESIAN_POINT ( 'NONE',  ( 1.071796769724492338, 28.50759618943233775, 12.99999999999999467 ) ) ;
#3898 = DIRECTION ( 'NONE',  ( 1.000000000000000000, 0.000000000000000000, 0.000000000000000000 ) ) ;
#3899 = CARTESIAN_POINT ( 'NONE',  ( 15.28000806814115720, 20.59240282405983535, 8.999999999999992895 ) ) ;
#3900 = CARTESIAN_POINT ( 'NONE',  ( 18.03564233677035844, 18.03564233677029094, 4.381197846482986158 ) ) ;
#3901 = ORIENTED_EDGE ( 'NONE', *, *, #21565, .T. ) ;
#3902 = DIRECTION ( 'NONE',  ( 1.000000000000000000, -2.891205793294678326E-16, 0.000000000000000000 ) ) ;
#3903 = CARTESIAN_POINT ( 'NONE',  ( 5.201626763664007669, 38.97563867572937824, 7.138217499902562935 ) ) ;
#3904 = CARTESIAN_POINT ( 'NONE',  ( 2.672651547586948120E-15, 27.84062499938548640, 13.33755215474602984 ) ) ;
#3905 = CARTESIAN_POINT ( 'NONE',  ( 19.00660103559776459, 17.49085150774564923, 12.99999999999999112 ) ) ;
#3906 = ADVANCED_FACE ( 'NONE', ( #19237 ), #5254, .F. ) ;
#3907 = PRESENTATION_LAYER_ASSIGNMENT (  '', '', ( #12686 ) ) ;
#3908 = CARTESIAN_POINT ( 'NONE',  ( 31.10000000000000142, -1.085850696380214537E-13, -6.500000000000000000 ) ) ;
#3909 = FACE_BOUND ( 'NONE', #19795, .T. ) ;
#3910 = ORIENTED_EDGE ( 'NONE', *, *, #10251, .T. ) ;
#3911 = CARTESIAN_POINT ( 'NONE',  ( 2.000000000000000888, 27.11874999877096926, 12.46410161513774817 ) ) ;
#3912 = LINE ( 'NONE', #6001, #12955 ) ;
#3914 = ORIENTED_EDGE ( 'NONE', *, *, #1319, .T. ) ;
#3913 = DIRECTION ( 'NONE',  ( 1.000000000000000000, 0.000000000000000000, 0.000000000000000000 ) ) ;
#3915 = MECHANICAL_DESIGN_GEOMETRIC_PRESENTATION_REPRESENTATION (  '', ( #3072 ), #10585 ) ;
#3916 = ORIENTED_EDGE ( 'NONE', *, *, #11089, .T. ) ;
#3917 = VERTEX_POINT ( 'NONE', #17940 ) ;
#3918 = VERTEX_POINT ( 'NONE', #10207 ) ;
#3919 = CARTESIAN_POINT ( 'NONE',  ( 0.000000000000000000, 0.000000000000000000, -6.500000000000000000 ) ) ;
#3920 = CARTESIAN_POINT ( 'NONE',  ( -26.52310962334761868, -16.23990935651689327, -2.750000000000000000 ) ) ;
#3921 = CARTESIAN_POINT ( 'NONE',  ( 6.009258394948636914E-15, 26.60312499938547859, 4.662447845253954171 ) ) ;
#3922 = CARTESIAN_POINT ( 'NONE',  ( 3.756430356250004099, -6.831223922626973533, 2.878124999385481608 ) ) ;
#3923 = CARTESIAN_POINT ( 'NONE',  ( -3.999999999999996003, -6.690598923241487306, 3.731249998770965970 ) ) ;
#3924 =( NAMED_UNIT ( * ) SI_UNIT ( $, .STERADIAN. ) SOLID_ANGLE_UNIT ( ) );
#3925 = EDGE_CURVE ( 'NONE', #22149, #21859, #6158, .T. ) ;
#3926 = CARTESIAN_POINT ( 'NONE',  ( 1.878215178125004048, 27.57812499938548711, 5.746835883940462963 ) ) ;
#3927 = EDGE_CURVE ( 'NONE', #18460, #2271, #3886, .T. ) ;
#3928 = CARTESIAN_POINT ( 'NONE',  ( 1.500000000000001776, -7.499999999999993783, 30.00000000000000355 ) ) ;
#3929 = CYLINDRICAL_SURFACE ( 'NONE', #3839, 0.5000000000000004441 ) ;
#3930 = CARTESIAN_POINT ( 'NONE',  ( 2.000000000000000888, -12.46410161513774817, 2.624999999999998668 ) ) ;
#3931 = DIRECTION ( 'NONE',  ( 0.000000000000000000, 0.000000000000000000, 1.000000000000000000 ) ) ;
#3932 = DIRECTION ( 'NONE',  ( 0.000000000000000000, -1.000000000000000000, 0.000000000000000000 ) ) ;
#3933 = DIRECTION ( 'NONE',  ( 0.000000000000000000, 0.000000000000000000, 1.000000000000000000 ) ) ;
#3934 = CARTESIAN_POINT ( 'NONE',  ( -2.000000000000000888, -29.36874999877096926, 12.46410161513774817 ) ) ;
#3935 = EDGE_CURVE ( 'NONE', #9796, #25585, #21733, .T. ) ;
#3936 = CARTESIAN_POINT ( 'NONE',  ( -3.756430356249997882, 27.76562499938549067, 11.16877607737301226 ) ) ;
#3937 = DIRECTION ( 'NONE',  ( 0.000000000000000000, -0.000000000000000000, 1.000000000000000000 ) ) ;
#3938 = ADVANCED_FACE ( 'NONE', ( #19773 ), #30, .T. ) ;
#3939 = DIRECTION ( 'NONE',  ( 0.000000000000000000, 0.000000000000000000, -1.000000000000000000 ) ) ;
#3940 = FACE_OUTER_BOUND ( 'NONE', #17928, .T. ) ;
#3941 = ORIENTED_EDGE ( 'NONE', *, *, #18233, .F. ) ;
#3942 = LINE ( 'NONE', #4191, #1651 ) ;
#3944 = ORIENTED_EDGE ( 'NONE', *, *, #4797, .T. ) ;
#3943 = CARTESIAN_POINT ( 'NONE',  ( 1.071796769724494558, 28.24240381056766580, 4.999999999999992895 ) ) ;
#3945 = ORIENTED_EDGE ( 'NONE', *, *, #14074, .T. ) ;
#3946 = CARTESIAN_POINT ( 'NONE',  ( 3.469446951953614189E-15, -8.999999999999992895, 0.000000000000000000 ) ) ;
#3947 = AXIS2_PLACEMENT_3D ( 'NONE', #19346, #19085, #23150 ) ;
#3948 = VERTEX_POINT ( 'NONE', #18206 ) ;
#3949 = CARTESIAN_POINT ( 'NONE',  ( -3.756430356250003655, -29.30312499938548498, 8.999999999999992895 ) ) ;
#3950 = ORIENTED_EDGE ( 'NONE', *, *, #25431, .F. ) ;
#3951 = ORIENTED_EDGE ( 'NONE', *, *, #2122, .T. ) ;
#3952 = CARTESIAN_POINT ( 'NONE',  ( -3.999999999999996447, -8.999999999999992895, 3.768749998770966947 ) ) ;
#3953 = ORIENTED_EDGE ( 'NONE', *, *, #19939, .F. ) ;
#3954 = CARTESIAN_POINT ( 'NONE',  ( 0.7500000000000001110, 0.000000000000000000, 17.69999999999999929 ) ) ;
#3955 = CARTESIAN_POINT ( 'NONE',  ( 2.672651547586948120E-15, 26.04062499938548925, 13.33755215474603162 ) ) ;
#3956 = CARTESIAN_POINT ( 'NONE',  ( 3.756430356250004099, -6.831223922626973533, 0.2906249993854818081 ) ) ;
#3957 = CARTESIAN_POINT ( 'NONE',  ( 23.01025686871646059, 20.92219106202042056, -2.750000000000000000 ) ) ;
#3958 = CARTESIAN_POINT ( 'NONE',  ( 17.90514199329621903, 23.21753674921489008, 8.999999999999992895 ) ) ;
#3959 = DIRECTION ( 'NONE',  ( 0.000000000000000000, 0.000000000000000000, -1.000000000000000000 ) ) ;
#3960 = EDGE_CURVE ( 'NONE', #18350, #23781, #16113, .T. ) ;
#3961 = CARTESIAN_POINT ( 'NONE',  ( 0.000000000000000000, 0.000000000000000000, 1.000000000000000000 ) ) ;
#3962 = SHAPE_DEFINITION_REPRESENTATION ( #16341, #22515 ) ;
#3963 = CARTESIAN_POINT ( 'NONE',  ( -3.999999999999996003, 27.88750000000000284, 6.690598923241487306 ) ) ;
#3964 = CARTESIAN_POINT ( 'NONE',  ( 3.756430356250002323, -11.16877607737301403, 0.6656249993854835845 ) ) ;
#3965 = CARTESIAN_POINT ( 'NONE',  ( -26.50000000000000355, -0.5000000000000000000, 19.50000000000000000 ) ) ;
#3966 = CARTESIAN_POINT ( 'NONE',  ( 1.071796769724497222, 28.05759618943234202, 12.99999999999998757 ) ) ;
#3967 = EDGE_LOOP ( 'NONE', ( #16984, #17177, #13654, #12427 ) ) ;
#3968 = ORIENTED_EDGE ( 'NONE', *, *, #17877, .F. ) ;
#3969 = CARTESIAN_POINT ( 'NONE',  ( -3.756430356249997882, 25.92812499938548854, 8.999999999999992895 ) ) ;
#3970 = EDGE_CURVE ( 'NONE', #14942, #16234, #16337, .T. ) ;
#3971 = ORIENTED_EDGE ( 'NONE', *, *, #17605, .T. ) ;
#3972 = CARTESIAN_POINT ( 'NONE',  ( -1.071796769724487230, 25.97634618820330132, 4.999999999999992006 ) ) ;
#3973 = CARTESIAN_POINT ( 'NONE',  ( 2.000000000000000888, 29.81874999877096855, 12.46410161513774817 ) ) ;
#3974 = CARTESIAN_POINT ( 'NONE',  ( 17.61017577620189556, 19.12592530405386526, 4.999999999999991118 ) ) ;
#3975 = CARTESIAN_POINT ( 'NONE',  ( 17.91631806831418317, 17.91631806831411566, 12.99999999999999289 ) ) ;
#3976 = ORIENTED_EDGE ( 'NONE', *, *, #15921, .T. ) ;
#3977 = VECTOR ( 'NONE', #8098, 1000.000000000000000 ) ;
#3978 = CARTESIAN_POINT ( 'NONE',  ( 5.577813053751546416E-15, 25.95624999877097139, 4.999999999999992006 ) ) ;
#3979 = ORIENTED_EDGE ( 'NONE', *, *, #18962, .T. ) ;
#3980 = FACE_OUTER_BOUND ( 'NONE', #10297, .T. ) ;
#3981 = CARTESIAN_POINT ( 'NONE',  ( 1.878215178125000939, 26.41562499938548214, 12.25316411605952283 ) ) ;
#3982 = CARTESIAN_POINT ( 'NONE',  ( 6.009258394948636914E-15, 27.50312499938549138, 4.662447845253954171 ) ) ;
#3983 = CARTESIAN_POINT ( 'NONE',  ( 21.21320343559646915, 21.21320343559638744, 8.999999999999992895 ) ) ;
#3984 = CARTESIAN_POINT ( 'NONE',  ( 2.000000000000005329, 28.22500000000000497, 5.535898384862238508 ) ) ;
#3985 = CARTESIAN_POINT ( 'NONE',  ( 3.735045420075836212E-15, 26.60312499938547859, 4.662447845253954171 ) ) ;
#3986 = CARTESIAN_POINT ( 'NONE',  ( -17.78012134629558716, 25.16042852506110705, -6.500000000000000000 ) ) ;
#3987 = LINE ( 'NONE', #7781, #11324 ) ;
#3988 = EDGE_CURVE ( 'NONE', #6294, #5290, #8005, .T. ) ;
#3989 = CARTESIAN_POINT ( 'NONE',  ( -27.25313774936397948, 14.98253926456367502, 1.000000000000000000 ) ) ;
#3990 = CARTESIAN_POINT ( 'NONE',  ( 18.59690834520624136, 21.42533546995235838, 5.535898384862237620 ) ) ;
#3991 = CARTESIAN_POINT ( 'NONE',  ( 23.66831732222138740, 18.35592256630256003, 11.16877607737301226 ) ) ;
#3992 = DIRECTION ( 'NONE',  ( 1.000000000000000000, 0.000000000000000000, 0.000000000000000000 ) ) ;
#3993 = DIRECTION ( 'NONE',  ( -0.000000000000000000, -1.000000000000000000, -0.000000000000000000 ) ) ;
#3994 = CARTESIAN_POINT ( 'NONE',  ( -5.840899737312982509, 31.50000000000000000, 7.627451181685283466 ) ) ;
#3995 = CARTESIAN_POINT ( 'NONE',  ( 0.000000000000000000, 0.000000000000000000, -6.500000000000000000 ) ) ;
#3996 = ORIENTED_EDGE ( 'NONE', *, *, #11092, .F. ) ;
#3997 = CARTESIAN_POINT ( 'NONE',  ( 4.000000000000001776, 27.60624999877096641, 11.30940107675849760 ) ) ;
#3998 = CARTESIAN_POINT ( 'NONE',  ( -2.000000000000000888, -27.62500000000000000, 12.46410161513774817 ) ) ;
#4000 = ORIENTED_EDGE ( 'NONE', *, *, #3267, .F. ) ;
#3999 = CARTESIAN_POINT ( 'NONE',  ( 1.878215178125003382, 26.67812499938548854, 5.746835883940462963 ) ) ;
#4001 = ADVANCED_FACE ( 'NONE', ( #10329 ), #6039, .F. ) ;
#4002 = CARTESIAN_POINT ( 'NONE',  ( -3.756430356249996105, 28.14062499938548356, 6.831223922626973533 ) ) ;
#4003 = CARTESIAN_POINT ( 'NONE',  ( 19.82388608118429119, 23.96296185032701587, 1.000000000000000000 ) ) ;
#4004 = CARTESIAN_POINT ( 'NONE',  ( 3.834746474454188013E-15, 28.26249999999999929, 4.999999999999992006 ) ) ;
#4005 = CARTESIAN_POINT ( 'NONE',  ( 2.000000000000003997, 26.36874999877096926, 5.535898384862238508 ) ) ;
#4006 = ORIENTED_EDGE ( 'NONE', *, *, #13171, .T. ) ;
#4007 = ORIENTED_EDGE ( 'NONE', *, *, #4182, .F. ) ;
#4008 = CARTESIAN_POINT ( 'NONE',  ( -3.756430356250003211, -25.29062499938548569, 6.831223922626973533 ) ) ;
#4009 = CARTESIAN_POINT ( 'NONE',  ( -3.756430356249996105, 26.67812499938548854, 6.831223922626973533 ) ) ;
#4010 = CARTESIAN_POINT ( 'NONE',  ( -3.756430356249996994, -8.999999999999992895, 4.415624999385483918 ) ) ;
#4011 = CARTESIAN_POINT ( 'NONE',  ( -15.41874213889376044, 27.00874656207322388, -6.500000000000000000 ) ) ;
#4012 = EDGE_CURVE ( 'NONE', #7798, #1111, #22606, .T. ) ;
#4013 = CARTESIAN_POINT ( 'NONE',  ( -1.999999999999998224, -12.46410161513774639, 3.900000000000000799 ) ) ;
#4014 = DIRECTION ( 'NONE',  ( -0.000000000000000000, -0.000000000000000000, -1.000000000000000000 ) ) ;
#4015 = ADVANCED_FACE ( 'NONE', ( #23822 ), #24205, .T. ) ;
#4016 = CYLINDRICAL_SURFACE ( 'NONE', #11732, 0.5000000000000004441 ) ;
#4017 = DIRECTION ( 'NONE',  ( 1.000000000000000000, 0.000000000000000000, 0.000000000000000000 ) ) ;
#4018 = CARTESIAN_POINT ( 'NONE',  ( 17.89864039878452928, 23.55549464827683437, 11.30940107675849404 ) ) ;
#4019 = CARTESIAN_POINT ( 'NONE',  ( 20.45982030258741702, 15.14742554666860208, 6.831223922626973533 ) ) ;
#4020 = CARTESIAN_POINT ( 'NONE',  ( 15.92316082797555055, 21.58001507746786274, 8.999999999999992895 ) ) ;
#4021 = ORIENTED_EDGE ( 'NONE', *, *, #15996, .F. ) ;
#4022 = CYLINDRICAL_SURFACE ( 'NONE', #2549, 0.5000000000000004441 ) ;
#4023 = CARTESIAN_POINT ( 'NONE',  ( -3.756430356249995661, 28.14062499938548356, 6.831223922626973533 ) ) ;
#4025 = ADVANCED_FACE ( 'NONE', ( #418 ), #5770, .T. ) ;
#4024 = LINE ( 'NONE', #24681, #14557 ) ;
#4026 = CARTESIAN_POINT ( 'NONE',  ( 4.000000000000003553, 25.19687499938548569, 8.999999999999992895 ) ) ;
#4027 = CARTESIAN_POINT ( 'NONE',  ( 29.09636799667079288, 10.98232076577223637, 1.000000000000000000 ) ) ;
#4028 = EDGE_LOOP ( 'NONE', ( #14703, #25556, #5591, #20296 ) ) ;
#4029 = PLANE ( 'NONE',  #25126 ) ;
#4030 = CARTESIAN_POINT ( 'NONE',  ( 4.000000000000003553, 25.88124999877096499, 6.690598923241489970 ) ) ;
#4031 = DIRECTION ( 'NONE',  ( 0.000000000000000000, 0.000000000000000000, 1.000000000000000000 ) ) ;
#4033 = ORIENTED_EDGE ( 'NONE', *, *, #4034, .T. ) ;
#4032 = CARTESIAN_POINT ( 'NONE',  ( 4.000000000000002665, 28.50624999877097210, 11.30940107675849760 ) ) ;
#4034 = EDGE_CURVE ( 'NONE', #25772, #10674, #25278, .T. ) ;
#4035 = VERTEX_POINT ( 'NONE', #3952 ) ;
#4036 = ORIENTED_EDGE ( 'NONE', *, *, #3848, .F. ) ;
#4037 = ADVANCED_FACE ( 'NONE', ( #11917 ), #12827, .F. ) ;
#4038 = VERTEX_POINT ( 'NONE', #2883 ) ;
#4039 = DIRECTION ( 'NONE',  ( 0.000000000000000000, 0.000000000000000000, 1.000000000000000000 ) ) ;
#4040 = CARTESIAN_POINT ( 'NONE',  ( -3.118462878979592734, 38.97860908142764913, 13.55684613422404006 ) ) ;
#4041 = CARTESIAN_POINT ( 'NONE',  ( -3.756430356249998326, 27.20312499938549067, 11.16877607737301226 ) ) ;
#4042 = CARTESIAN_POINT ( 'NONE',  ( 3.756430356250003655, -8.999999999999992895, 4.640624999385483562 ) ) ;
#4043 = CARTESIAN_POINT ( 'NONE',  ( 2.620986760973688460E-15, -13.61880215351699874, 4.781249998770965348 ) ) ;
#4044 = CARTESIAN_POINT ( 'NONE',  ( -3.756430356249996994, 25.81562499938548427, 8.999999999999992895 ) ) ;
#4045 = DIRECTION ( 'NONE',  ( 0.000000000000000000, 0.000000000000000000, 1.000000000000000000 ) ) ;
#4046 = DIRECTION ( 'NONE',  ( 0.5877852522924853496, 0.8090169943749385695, 0.000000000000000000 ) ) ;
#4047 = CARTESIAN_POINT ( 'NONE',  ( -1.878215178124998497, 27.24062499938548498, 12.25316411605951927 ) ) ;
#4048 = DIRECTION ( 'NONE',  ( 0.000000000000000000, 0.000000000000000000, -1.000000000000000000 ) ) ;
#4049 = CARTESIAN_POINT ( 'NONE',  ( 1.999999999999998224, -25.69374999877097210, 12.46410161513774639 ) ) ;
#4050 = CARTESIAN_POINT ( 'NONE',  ( 1.580380365229604700E-14, 27.58750000000000213, 12.99999999999999289 ) ) ;
#4051 = CARTESIAN_POINT ( 'NONE',  ( -4.000000000000001776, -28.95624999877097494, 11.30940107675849760 ) ) ;
#4052 = CARTESIAN_POINT ( 'NONE',  ( -1.878215178124998497, 28.25312499938548427, 12.25316411605951927 ) ) ;
#4053 = DIRECTION ( 'NONE',  ( 1.000000000000000000, 0.000000000000000000, 0.000000000000000000 ) ) ;
#4054 = FACE_OUTER_BOUND ( 'NONE', #11297, .T. ) ;
#4055 = CARTESIAN_POINT ( 'NONE',  ( -30.78811501957148167, -4.393401135980793626, -6.500000000000000000 ) ) ;
#4056 = ORIENTED_EDGE ( 'NONE', *, *, #20696, .F. ) ;
#4057 = CARTESIAN_POINT ( 'NONE',  ( 4.000000000000003553, 28.63749999999999929, 6.690598923241489970 ) ) ;
#4059 = ORIENTED_EDGE ( 'NONE', *, *, #8340, .F. ) ;
#4058 = CARTESIAN_POINT ( 'NONE',  ( 2.000000000000000888, 28.07500000000000284, 12.46410161513774817 ) ) ;
#4060 = ORIENTED_EDGE ( 'NONE', *, *, #5161, .F. ) ;
#4061 = FACE_OUTER_BOUND ( 'NONE', #14921, .T. ) ;
#4062 = ORIENTED_EDGE ( 'NONE', *, *, #3370, .F. ) ;
#4063 = ADVANCED_FACE ( 'NONE', ( #18465 ), #2637, .T. ) ;
#4064 = ORIENTED_EDGE ( 'NONE', *, *, #20094, .T. ) ;
#4065 = VERTEX_POINT ( 'NONE', #8918 ) ;
#4066 = CARTESIAN_POINT ( 'NONE',  ( 22.70696651085303941, 17.05011226136058866, 11.30940107675849760 ) ) ;
#4067 = EDGE_CURVE ( 'NONE', #9149, #21754, #4679, .T. ) ;
#4068 = ORIENTED_EDGE ( 'NONE', *, *, #7872, .F. ) ;
#4069 = DIRECTION ( 'NONE',  ( 1.000000000000000000, 0.000000000000000000, 0.000000000000000000 ) ) ;
#4070 = CARTESIAN_POINT ( 'NONE',  ( -3.756430356249996105, 25.89062499938548356, 6.831223922626973533 ) ) ;
#4071 = FACE_OUTER_BOUND ( 'NONE', #10750, .T. ) ;
#4072 = DIRECTION ( 'NONE',  ( 0.000000000000000000, 0.000000000000000000, 1.000000000000000000 ) ) ;
#4073 = CARTESIAN_POINT ( 'NONE',  ( 17.19146985159974150, 19.84766722955904683, 5.746835883940462963 ) ) ;
#4074 = DIRECTION ( 'NONE',  ( 0.000000000000000000, 0.000000000000000000, 1.000000000000000000 ) ) ;
#4075 = CYLINDRICAL_SURFACE ( 'NONE', #865, 4.000000000000000000 ) ;
#4076 = AXIS2_PLACEMENT_3D ( 'NONE', #25290, #980, #13395 ) ;
#4077 = CARTESIAN_POINT ( 'NONE',  ( -1.878215178124995832, -5.746835883940462963, 1.640624999385484450 ) ) ;
#4078 = CARTESIAN_POINT ( 'NONE',  ( -3.999999999999996447, 28.37500000000000000, 8.999999999999992895 ) ) ;
#4079 = CARTESIAN_POINT ( 'NONE',  ( 4.000000000000003553, 29.05000000000000071, 8.999999999999992895 ) ) ;
#4080 = CARTESIAN_POINT ( 'NONE',  ( 3.469446951953614189E-15, 35.50000000000000711, 8.999999999999992895 ) ) ;
#4081 = CARTESIAN_POINT ( 'NONE',  ( 22.74023967191403628, 17.42784491599521601, 8.999999999999992895 ) ) ;
#4082 = CARTESIAN_POINT ( 'NONE',  ( 22.67092431280594056, 21.28941499438218088, -6.500000000000000000 ) ) ;
#4083 = ORIENTED_EDGE ( 'NONE', *, *, #24665, .F. ) ;
#4084 = ORIENTED_EDGE ( 'NONE', *, *, #2780, .T. ) ;
#4085 = CARTESIAN_POINT ( 'NONE',  ( 3.756430356250004987, 26.60312499938548569, 8.999999999999992895 ) ) ;
#4086 = ORIENTED_EDGE ( 'NONE', *, *, #10046, .F. ) ;
#4087 = LINE ( 'NONE', #7639, #7909 ) ;
#4088 = EDGE_CURVE ( 'NONE', #12917, #3948, #6942, .T. ) ;
#4089 = CARTESIAN_POINT ( 'NONE',  ( 2.672651547586948120E-15, 26.04062499938548925, 13.33755215474602984 ) ) ;
#4090 = CARTESIAN_POINT ( 'NONE',  ( 3.756430356250003655, 29.75312499938548783, 8.999999999999992895 ) ) ;
#4091 = CARTESIAN_POINT ( 'NONE',  ( 3.752267015613588906E-15, -4.381197846482986158, 2.306249998770968368 ) ) ;
#4092 = VERTEX_POINT ( 'NONE', #4732 ) ;
#4093 = EDGE_CURVE ( 'NONE', #17423, #10079, #18848, .T. ) ;
#4094 = AXIS2_PLACEMENT_3D ( 'NONE', #22666, #20566, #10616 ) ;
#4095 = CARTESIAN_POINT ( 'NONE',  ( -1.859271017917182139E-15, -25.78750000000000142, 12.99999999999999289 ) ) ;
#4096 = ORIENTED_EDGE ( 'NONE', *, *, #14893, .T. ) ;
#4097 = DIRECTION ( 'NONE',  ( 0.000000000000000000, -1.000000000000000000, 0.000000000000000000 ) ) ;
#4098 = CARTESIAN_POINT ( 'NONE',  ( 1.878215178125004048, 27.46562499938548640, 5.746835883940462963 ) ) ;
#4099 =( BOUNDED_CURVE ( )  B_SPLINE_CURVE ( 2, ( #3575, #17709, #11546, #21753, #19513, #15618, #9586, #50, #1758 ),
 .UNSPECIFIED., .F., .F. ) 
 B_SPLINE_CURVE_WITH_KNOTS ( ( 3, 2, 2, 2, 3 ),
 ( 0.8750000000000000000, 0.8833333333333333037, 0.9000000000000000222, 0.9166666666666666297, 0.9250000000000000444 ),
 .UNSPECIFIED. ) 
 CURVE ( )  GEOMETRIC_REPRESENTATION_ITEM ( )  RATIONAL_B_SPLINE_CURVE ( ( 0.9330127018922194093, 0.9330127018922194093, 1.000000000000000000, 0.8660254037844387076, 1.000000000000000000, 0.8660254037844387076, 1.000000000000000000, 0.9330127018922189652, 0.9330127018922194093 ) ) 
 REPRESENTATION_ITEM ( '' )  );
#4100 = CARTESIAN_POINT ( 'NONE',  ( 3.756430356250002323, 29.60312499938548925, 11.16877607737301403 ) ) ;
#4101 = CARTESIAN_POINT ( 'NONE',  ( -26.52310962334761868, -16.23990935651689327, -6.500000000000000000 ) ) ;
#4102 = CARTESIAN_POINT ( 'NONE',  ( 4.000000000000003553, -8.999999999999992895, 18.00000000000000000 ) ) ;
#4103 = CARTESIAN_POINT ( 'NONE',  ( -3.999999999999996447, 28.33750000000000568, 6.690598923241487306 ) ) ;
#4104 = EDGE_CURVE ( 'NONE', #3462, #10049, #10599, .T. ) ;
#4105 = EDGE_CURVE ( 'NONE', #4358, #20170, #4738, .T. ) ;
#4106 = CARTESIAN_POINT ( 'NONE',  ( 2.672651547586948120E-15, 25.92812499938548498, 13.33755215474602984 ) ) ;
#4107 = DIRECTION ( 'NONE',  ( 1.000000000000000000, 0.000000000000000000, 0.000000000000000000 ) ) ;
#4108 = AXIS2_PLACEMENT_3D ( 'NONE', #4443, #14131, #4720 ) ;
#4109 = VECTOR ( 'NONE', #3241, 1000.000000000000000 ) ;
#4110 = DIRECTION ( 'NONE',  ( 0.000000000000000000, 0.000000000000000000, 1.000000000000000000 ) ) ;
#4111 = CARTESIAN_POINT ( 'NONE',  ( -0.4972522109372425891, 38.55547752541761497, 3.076310858750954225 ) ) ;
#4112 = FACE_OUTER_BOUND ( 'NONE', #1765, .T. ) ;
#4113 = CARTESIAN_POINT ( 'NONE',  ( 0.5000000000000000000, 0.8660254037844387076, 20.00000000000000000 ) ) ;
#4115 = CARTESIAN_POINT ( 'NONE',  ( -2.672651547586948120E-15, -25.47812499938548569, 13.33755215474603162 ) ) ;
#4114 = AXIS2_PLACEMENT_3D ( 'NONE', #18804, #20639, #14885 ) ;
#4116 = CARTESIAN_POINT ( 'NONE',  ( 22.95237170627000367, 17.63997695035117985, 11.16877607737301403 ) ) ;
#4117 = AXIS2_PLACEMENT_3D ( 'NONE', #6724, #14193, #12089 ) ;
#4118 = ORIENTED_EDGE ( 'NONE', *, *, #9299, .F. ) ;
#4119 = CARTESIAN_POINT ( 'NONE',  ( 2.000000000000000888, 28.01874999877096784, 12.46410161513774817 ) ) ;
#4120 = CARTESIAN_POINT ( 'NONE',  ( -2.620986760973688460E-15, -28.93750000000000000, 13.61880215351699874 ) ) ;
#4122 = VERTEX_POINT ( 'NONE', #796 ) ;
#4121 = CARTESIAN_POINT ( 'NONE',  ( 3.756430356250004987, 26.60312499938548569, 8.999999999999992895 ) ) ;
#4123 = EDGE_CURVE ( 'NONE', #22108, #1305, #4979, .T. ) ;
#4124 = CARTESIAN_POINT ( 'NONE',  ( -1.878215178124995832, 28.55312499938548498, 5.746835883940462963 ) ) ;
#4125 = CARTESIAN_POINT ( 'NONE',  ( -21.65113613650310143, 22.32573188046944068, -2.750000000000000000 ) ) ;
#4126 = DIRECTION ( 'NONE',  ( -0.000000000000000000, -1.000000000000000000, -0.000000000000000000 ) ) ;
#4127 = ORIENTED_EDGE ( 'NONE', *, *, #18605, .F. ) ;
#4128 = ORIENTED_EDGE ( 'NONE', *, *, #21854, .T. ) ;
#4129 = CARTESIAN_POINT ( 'NONE',  ( 3.756430356249997438, -25.51562499938548356, 11.16877607737301048 ) ) ;
#4130 = CARTESIAN_POINT ( 'NONE',  ( -1.878215178124998275, 27.24062499938548854, 12.25316411605951927 ) ) ;
#4131 = LINE ( 'NONE', #8196, #11782 ) ;
#4132 = EDGE_CURVE ( 'NONE', #13061, #6542, #22893, .T. ) ;
#4133 = CIRCLE ( 'NONE', #18752, 0.5000000000000000000 ) ;
#4134 = CARTESIAN_POINT ( 'NONE',  ( 3.735045420075836212E-15, -4.662447845253954171, 3.403124999385482408 ) ) ;
#4135 = CIRCLE ( 'NONE', #18757, 0.5000000000000005551 ) ;
#4136 = ADVANCED_FACE ( 'NONE', ( #3023 ), #18976, .T. ) ;
#4137 = AXIS2_PLACEMENT_3D ( 'NONE', #3806, #8247, #18313 ) ;
#4138 = CARTESIAN_POINT ( 'NONE',  ( -3.999999999999996447, 27.41874999877096641, 8.999999999999992895 ) ) ;
#4139 = SURFACE_SIDE_STYLE ('',( #6368 ) ) ;
#4140 = DIRECTION ( 'NONE',  ( 1.000000000000000000, 0.000000000000000000, 0.000000000000000000 ) ) ;
#4141 = CARTESIAN_POINT ( 'NONE',  ( 17.80583263288473717, 23.46268688237703870, 6.690598923241487306 ) ) ;
#4142 = LINE ( 'NONE', #13968, #1746 ) ;
#4143 = CARTESIAN_POINT ( 'NONE',  ( 19.63547142920491595, 16.80704430445866393, 12.46410161513774817 ) ) ;
#4144 = DIRECTION ( 'NONE',  ( 0.000000000000000000, 0.000000000000000000, -1.000000000000000000 ) ) ;
#4145 = CARTESIAN_POINT ( 'NONE',  ( -3.137519842735244810E-15, 26.46249999999999858, 4.999999999999991118 ) ) ;
#4146 = CARTESIAN_POINT ( 'NONE',  ( 17.85886564147372724, 23.51571989096603232, 11.30940107675849404 ) ) ;
#4147 = EDGE_LOOP ( 'NONE', ( #25523, #16815, #25214, #3046, #1987 ) ) ;
#4148 = CARTESIAN_POINT ( 'NONE',  ( 1.071796769724485454, -27.11740381056766580, 12.99999999999999467 ) ) ;
#4149 = PLANE ( 'NONE',  #7144 ) ;
#4150 = CARTESIAN_POINT ( 'NONE',  ( -3.756430356249997882, 29.56562499938549138, 11.16877607737301226 ) ) ;
#4151 = AXIS2_PLACEMENT_3D ( 'NONE', #4401, #14740, #24927 ) ;
#4152 = CARTESIAN_POINT ( 'NONE',  ( -14.54246377227378062, -27.49048467073843227, -6.500000000000000000 ) ) ;
#4153 = AXIS2_PLACEMENT_3D ( 'NONE', #19347, #6809, #10986 ) ;
#4154 = CARTESIAN_POINT ( 'NONE',  ( -1.999999999999996669, 26.20000000000000639, 12.46410161513774639 ) ) ;
#4155 = DIRECTION ( 'NONE',  ( 0.000000000000000000, 0.000000000000000000, 1.000000000000000000 ) ) ;
#4156 = ORIENTED_EDGE ( 'NONE', *, *, #7037, .F. ) ;
#4157 = DIRECTION ( 'NONE',  ( -1.000000000000000000, 0.000000000000000000, 0.000000000000000000 ) ) ;
#4158 = CARTESIAN_POINT ( 'NONE',  ( 4.000000000000003553, 26.29374999877096997, 8.999999999999992895 ) ) ;
#4159 = CARTESIAN_POINT ( 'NONE',  ( -3.756430356250003655, -25.14062499938548356, 8.999999999999992895 ) ) ;
#4161 = ORIENTED_EDGE ( 'NONE', *, *, #15136, .F. ) ;
#4160 = FACE_OUTER_BOUND ( 'NONE', #22009, .T. ) ;
#4162 = CIRCLE ( 'NONE', #20021, 31.10000000000000142 ) ;
#4163 = ORIENTED_EDGE ( 'NONE', *, *, #6994, .T. ) ;
#4164 = EDGE_LOOP ( 'NONE', ( #4127, #21755, #12241, #24038 ) ) ;
#4165 = EDGE_LOOP ( 'NONE', ( #20942, #15306, #17453, #9056 ) ) ;
#4166 = DIRECTION ( 'NONE',  ( 1.000000000000000000, 0.000000000000000000, 0.000000000000000000 ) ) ;
#4167 = CARTESIAN_POINT ( 'NONE',  ( 13.24173596767378847, 28.14012133169319796, -6.500000000000000000 ) ) ;
#4168 = EDGE_CURVE ( 'NONE', #22990, #21593, #24316, .T. ) ;
#4169 = AXIS2_PLACEMENT_3D ( 'NONE', #18197, #9823, #158 ) ;
#4170 = CARTESIAN_POINT ( 'NONE',  ( 6.009258394948636914E-15, 27.95312499938548356, 4.662447845253954171 ) ) ;
#4171 = AXIS2_PLACEMENT_3D ( 'NONE', #12838, #15070, #20956 ) ;
#4172 = EDGE_CURVE ( 'NONE', #20797, #12699, #527, .T. ) ;
#4173 = DIRECTION ( 'NONE',  ( 0.000000000000000000, 0.000000000000000000, 1.000000000000000000 ) ) ;
#4174 = CARTESIAN_POINT ( 'NONE',  ( -3.756430356249997882, -11.16877607737301226, 0.5156249993854836733 ) ) ;
#4175 = CARTESIAN_POINT ( 'NONE',  ( 3.756430356250002323, 25.55312499938548143, 11.16877607737301226 ) ) ;
#4176 = VECTOR ( 'NONE', #2507, 1000.000000000000000 ) ;
#4177 = DIRECTION ( 'NONE',  ( -0.000000000000000000, -1.000000000000000000, -0.000000000000000000 ) ) ;
#4178 = FACE_OUTER_BOUND ( 'NONE', #6188, .T. ) ;
#4179 = CARTESIAN_POINT ( 'NONE',  ( 3.756430356250002323, 26.45312499938548356, 11.16877607737301403 ) ) ;
#4180 = DIRECTION ( 'NONE',  ( 1.000000000000000000, 0.000000000000000000, 0.000000000000000000 ) ) ;
#4182 = EDGE_CURVE ( 'NONE', #2494, #5410, #20544, .T. ) ;
#4181 = CARTESIAN_POINT ( 'NONE',  ( -3.063240906311874401, -29.84319947910909931, 11.57226653943512851 ) ) ;
#4183 = CARTESIAN_POINT ( 'NONE',  ( -3.999999999999995559, 28.73124999877096997, 6.690598923241487306 ) ) ;
#4184 = CARTESIAN_POINT ( 'NONE',  ( -2.000000000000000888, -29.81874999877096855, 12.46410161513774817 ) ) ;
#4185 = CARTESIAN_POINT ( 'NONE',  ( -1.878215178124998497, 29.15312499938548640, 12.25316411605951927 ) ) ;
#4186 = CARTESIAN_POINT ( 'NONE',  ( -1.071796769724487230, 27.83259618943233704, 4.999999999999992006 ) ) ;
#4187 = CIRCLE ( 'NONE', #18814, 31.10000000000000142 ) ;
#4188 = CARTESIAN_POINT ( 'NONE',  ( -3.999999999999982681, -11.30940107675850292, 1.612499999999998490 ) ) ;
#4189 = DIRECTION ( 'NONE',  ( -0.000000000000000000, -1.000000000000000000, -0.000000000000000000 ) ) ;
#4190 = ORIENTED_EDGE ( 'NONE', *, *, #21931, .T. ) ;
#4191 = CARTESIAN_POINT ( 'NONE',  ( 28.34936733434196299, -12.78762572734067149, -2.750000000000000000 ) ) ;
#4193 = ORIENTED_EDGE ( 'NONE', *, *, #17399, .F. ) ;
#4192 = DIRECTION ( 'NONE',  ( 0.000000000000000000, 0.000000000000000000, 1.000000000000000000 ) ) ;
#4194 = VECTOR ( 'NONE', #16741, 1000.000000000000000 ) ;
#4195 = VERTEX_POINT ( 'NONE', #24470 ) ;
#4196 = ORIENTED_EDGE ( 'NONE', *, *, #10386, .T. ) ;
#4197 = EDGE_CURVE ( 'NONE', #3025, #1894, #12706, .T. ) ;
#4198 = ORIENTED_EDGE ( 'NONE', *, *, #2345, .T. ) ;
#4199 = EDGE_LOOP ( 'NONE', ( #20046, #18620, #9848, #6177 ) ) ;
#4200 = DIRECTION ( 'NONE',  ( 0.7289686274214236539, 0.6845471059286760696, 0.000000000000000000 ) ) ;
#4201 =( GEOMETRIC_REPRESENTATION_CONTEXT ( 3 ) GLOBAL_UNCERTAINTY_ASSIGNED_CONTEXT ( ( #23009 ) ) GLOBAL_UNIT_ASSIGNED_CONTEXT ( ( #22125, #4213, #24359 ) ) REPRESENTATION_CONTEXT ( 'NONE', 'WORKASPACE' ) );
#4202 = VERTEX_POINT ( 'NONE', #20676 ) ;
#4203 = CARTESIAN_POINT ( 'NONE',  ( -1.999999999999995781, 28.75000000000000000, 5.535898384862237620 ) ) ;
#4204 = CARTESIAN_POINT ( 'NONE',  ( 3.756430356250003655, 26.15312499938548640, 8.999999999999992895 ) ) ;
#4205 = CIRCLE ( 'NONE', #8806, 0.7500000000000001110 ) ;
#4206 = CARTESIAN_POINT ( 'NONE',  ( 2.672651547586948120E-15, -13.33755215474602984, 1.490624999385481209 ) ) ;
#4207 = DIRECTION ( 'NONE',  ( 0.6374239897486995154, 0.7705132427757811486, 0.000000000000000000 ) ) ;
#4208 = CARTESIAN_POINT ( 'NONE',  ( 16.89751483010538990, 22.20990958602406451, 11.16877607737301226 ) ) ;
#4209 = ADVANCED_FACE ( 'NONE', ( #2758 ), #22504, .F. ) ;
#4210 = AXIS2_PLACEMENT_3D ( 'NONE', #16704, #18929, #10671 ) ;
#4211 = CARTESIAN_POINT ( 'NONE',  ( 3.469446951953614189E-15, -8.999999999999992895, 18.00000000000000000 ) ) ;
#4212 = CIRCLE ( 'NONE', #11302, 0.4999999999999989453 ) ;
#4213 =( NAMED_UNIT ( * ) PLANE_ANGLE_UNIT ( ) SI_UNIT ( $, .RADIAN. ) );
#4214 = CARTESIAN_POINT ( 'NONE',  ( -3.756430356249995661, -6.831223922626973533, 1.678124999385481875 ) ) ;
#4215 = EDGE_CURVE ( 'NONE', #15212, #4065, #5121, .T. ) ;
#4216 = CARTESIAN_POINT ( 'NONE',  ( -1.999999999999998224, 28.00000000000000000, 12.46410161513774639 ) ) ;
#4217 = CARTESIAN_POINT ( 'NONE',  ( 3.756430356250003655, 29.19062499938548072, 8.999999999999992895 ) ) ;
#4219 = EDGE_CURVE ( 'NONE', #1228, #12953, #25497, .T. ) ;
#4218 = VECTOR ( 'NONE', #145, 1000.000000000000000 ) ;
#4220 = CARTESIAN_POINT ( 'NONE',  ( -30.78811501957138930, 4.393401135981437555, -6.500000000000000000 ) ) ;
#4221 = CARTESIAN_POINT ( 'NONE',  ( 3.834746474454188013E-15, 27.36250000000000426, 4.999999999999992006 ) ) ;
#4222 = CARTESIAN_POINT ( 'NONE',  ( -3.834746474454188013E-15, -28.26249999999999929, 4.999999999999992006 ) ) ;
#4223 = EDGE_LOOP ( 'NONE', ( #21183, #19561, #14384, #830 ) ) ;
#4224 = EDGE_LOOP ( 'NONE', ( #11720, #19596, #3950, #3707 ) ) ;
#4225 = CARTESIAN_POINT ( 'NONE',  ( 2.000000000000007105, 29.51874999877097139, 5.535898384862238508 ) ) ;
#4226 = ORIENTED_EDGE ( 'NONE', *, *, #22255, .F. ) ;
#4227 = DIRECTION ( 'NONE',  ( 0.000000000000000000, 0.000000000000000000, -1.000000000000000000 ) ) ;
#4228 = ORIENTED_EDGE ( 'NONE', *, *, #21940, .F. ) ;
#4229 = CARTESIAN_POINT ( 'NONE',  ( 4.000000000000012434, -6.690598923241494411, 2.231249998770966858 ) ) ;
#4230 = ORIENTED_EDGE ( 'NONE', *, *, #21894, .T. ) ;
#4231 = CIRCLE ( 'NONE', #6325, 2.000000000000000000 ) ;
#4232 = AXIS2_PLACEMENT_3D ( 'NONE', #4603, #22664, #20691 ) ;
#4233 = DIRECTION ( 'NONE',  ( 1.000000000000000000, 0.000000000000000000, 0.000000000000000000 ) ) ;
#4234 = EDGE_LOOP ( 'NONE', ( #5141, #21984, #15593, #9325 ) ) ;
#4235 = CARTESIAN_POINT ( 'NONE',  ( 21.21320343559646915, 21.21320343559638744, 8.999999999999992895 ) ) ;
#4236 = CARTESIAN_POINT ( 'NONE',  ( -3.756430356249996994, 28.06562499938548427, 8.999999999999992895 ) ) ;
#4237 = CARTESIAN_POINT ( 'NONE',  ( 2.000000000000000888, 28.97500000000000142, 12.46410161513774817 ) ) ;
#4238 = VECTOR ( 'NONE', #5982, 1000.000000000000000 ) ;
#4239 = CARTESIAN_POINT ( 'NONE',  ( 3.469446951953614189E-15, 39.50000000000000000, 8.999999999999992895 ) ) ;
#4240 = CARTESIAN_POINT ( 'NONE',  ( 0.000000000000000000, 0.000000000000000000, -6.500000000000000000 ) ) ;
#4241 = CARTESIAN_POINT ( 'NONE',  ( 4.000000000000002665, 28.56249999999999645, 11.30940107675849760 ) ) ;
#4242 = AXIS2_PLACEMENT_3D ( 'NONE', #22924, #5009, #12993 ) ;
#4243 = ADVANCED_FACE ( 'NONE', ( #11114 ), #17522, .T. ) ;
#4244 = CARTESIAN_POINT ( 'NONE',  ( 3.735045420075836212E-15, 25.25312499938548783, 4.662447845253954171 ) ) ;
#4245 = AXIS2_PLACEMENT_3D ( 'NONE', #22012, #12066, #20044 ) ;
#4246 = EDGE_CURVE ( 'NONE', #3783, #1051, #23475, .T. ) ;
#4247 = CIRCLE ( 'NONE', #19274, 0.5000000000000004441 ) ;
#4248 = DIRECTION ( 'NONE',  ( 0.000000000000000000, 0.000000000000000000, -1.000000000000000000 ) ) ;
#4249 = DIRECTION ( 'NONE',  ( 0.000000000000000000, 0.000000000000000000, -1.000000000000000000 ) ) ;
#4250 = CYLINDRICAL_SURFACE ( 'NONE', #16832, 30.10000000000000142 ) ;
#4251 = CARTESIAN_POINT ( 'NONE',  ( -22.67092431280563503, 21.28941499438250062, -6.500000000000000000 ) ) ;
#4252 =( BOUNDED_CURVE ( )  B_SPLINE_CURVE ( 2, ( #20654, #24839, #6794, #20374, #24959, #14899, #22872 ),
 .UNSPECIFIED., .F., .F. ) 
 B_SPLINE_CURVE_WITH_KNOTS ( ( 3, 2, 2, 3 ),
 ( 0.3000000000000002109, 0.3166666666666668184, 0.3333333333333334814, 0.3500000000000000888 ),
 .UNSPECIFIED. ) 
 CURVE ( )  GEOMETRIC_REPRESENTATION_ITEM ( )  RATIONAL_B_SPLINE_CURVE ( ( 0.9999999999999982236, 0.8660254037844404840, 1.000000000000000000, 0.8660254037844387076, 1.000000000000000000, 0.8660254037844378194, 1.000000000000000888 ) ) 
 REPRESENTATION_ITEM ( '' )  );
#4253 = EDGE_CURVE ( 'NONE', #18011, #18810, #24732, .T. ) ;
#4254 = CARTESIAN_POINT ( 'NONE',  ( 20.26302869750798408, 20.26302869750790947, 4.999999999999992006 ) ) ;
#4255 = CIRCLE ( 'NONE', #12189, 24.00000000000000355 ) ;
#4256 = CARTESIAN_POINT ( 'NONE',  ( 3.756430356249996994, -25.81562499938548427, 8.999999999999992895 ) ) ;
#4257 = CARTESIAN_POINT ( 'NONE',  ( 5.206848532682268882, 39.00010698140258825, 10.77302451745546286 ) ) ;
#4258 = ORIENTED_EDGE ( 'NONE', *, *, #11420, .T. ) ;
#4259 = CARTESIAN_POINT ( 'NONE',  ( -1.999999999999995781, 27.79374999877096997, 5.535898384862237620 ) ) ;
#4260 = CARTESIAN_POINT ( 'NONE',  ( 22.34899370200828983, 16.69213945251583908, 11.30940107675849760 ) ) ;
#4262 = ORIENTED_EDGE ( 'NONE', *, *, #17280, .F. ) ;
#4261 = CARTESIAN_POINT ( 'NONE',  ( -3.756430356249996549, 27.76562499938549422, 11.16877607737301048 ) ) ;
#4263 = ORIENTED_EDGE ( 'NONE', *, *, #7114, .F. ) ;
#4264 = CARTESIAN_POINT ( 'NONE',  ( -3.756430356249997438, 29.11562499938548498, 11.16877607737301048 ) ) ;
#4265 =( BOUNDED_CURVE ( )  B_SPLINE_CURVE ( 2, ( #6860, #22197, #21937, #22816, #6107, #843, #2200, #11868, #11983 ),
 .UNSPECIFIED., .F., .F. ) 
 B_SPLINE_CURVE_WITH_KNOTS ( ( 3, 2, 2, 2, 3 ),
 ( 0.07500000000000001110, 0.08333333333333332871, 0.1000000000000000056, 0.1166666666666666685, 0.1249999999999999861 ),
 .UNSPECIFIED. ) 
 CURVE ( )  GEOMETRIC_REPRESENTATION_ITEM ( )  RATIONAL_B_SPLINE_CURVE ( ( 0.9330127018922192983, 0.9330127018922194093, 1.000000000000000000, 0.8660254037844387076, 1.000000000000000000, 0.8660254037844387076, 1.000000000000000000, 0.9330127018922195203, 0.9330127018922194093 ) ) 
 REPRESENTATION_ITEM ( '' )  );
#4266 = VECTOR ( 'NONE', #24731, 1000.000000000000000 ) ;
#4267 = FACE_OUTER_BOUND ( 'NONE', #415, .T. ) ;
#4268 = LINE ( 'NONE', #10385, #11704 ) ;
#4269 = VERTEX_POINT ( 'NONE', #17400 ) ;
#4270 = VERTEX_POINT ( 'NONE', #23540 ) ;
#4271 = CARTESIAN_POINT ( 'NONE',  ( -1.878215178125004048, -26.22812499938548569, 5.746835883940462963 ) ) ;
#4272 = CIRCLE ( 'NONE', #3028, 0.5000000000000000000 ) ;
#4273 = CARTESIAN_POINT ( 'NONE',  ( -3.756430356249994773, 28.96562499938548640, 8.999999999999992895 ) ) ;
#4274 = CARTESIAN_POINT ( 'NONE',  ( 1.626862140677534194E-14, 27.98124999877096997, 12.99999999999999289 ) ) ;
#4275 = CARTESIAN_POINT ( 'NONE',  ( -3.756430356249996994, -8.999999999999992895, 2.615624999385480987 ) ) ;
#4276 = CARTESIAN_POINT ( 'NONE',  ( -3.999999999999995559, -6.690598923241487306, 3.337499999999999023 ) ) ;
#4277 = FILL_AREA_STYLE ('',( #15786 ) ) ;
#4278 = EDGE_CURVE ( 'NONE', #18972, #5285, #938, .T. ) ;
#4279 = LINE ( 'NONE', #110, #15026 ) ;
#4280 = ADVANCED_FACE ( 'NONE', ( #11504 ), #11623, .T. ) ;
#4281 = DIRECTION ( 'NONE',  ( 0.000000000000000000, -1.000000000000000000, 0.000000000000000000 ) ) ;
#4282 = AXIS2_PLACEMENT_3D ( 'NONE', #14890, #14632, #10817 ) ;
#4283 = CYLINDRICAL_SURFACE ( 'NONE', #5085, 31.10000000000000142 ) ;
#4284 = DIRECTION ( 'NONE',  ( 0.000000000000000000, 0.000000000000000000, 1.000000000000000000 ) ) ;
#4285 = CARTESIAN_POINT ( 'NONE',  ( 28.91604871112465602, 11.44867358849340633, 1.000000000000000000 ) ) ;
#4286 = CARTESIAN_POINT ( 'NONE',  ( 15.88988766691455368, 21.20228242283322828, 6.831223922626973533 ) ) ;
#4287 = CARTESIAN_POINT ( 'NONE',  ( 18.98139765660737055, 21.80982478135348757, 12.46410161513774639 ) ) ;
#4288 = VERTEX_POINT ( 'NONE', #5621 ) ;
#4289 = DIRECTION ( 'NONE',  ( 0.000000000000000000, 0.000000000000000000, -1.000000000000000000 ) ) ;
#4290 = DIRECTION ( 'NONE',  ( -0.000000000000000000, -0.000000000000000000, 1.000000000000000000 ) ) ;
#4291 = CARTESIAN_POINT ( 'NONE',  ( -3.756430356249995661, 29.49062499938548498, 6.831223922626973533 ) ) ;
#4292 = CIRCLE ( 'NONE', #21824, 1.000000000000000000 ) ;
#4294 = EDGE_LOOP ( 'NONE', ( #21564, #9350, #24727, #8153 ) ) ;
#4293 = DIRECTION ( 'NONE',  ( 0.000000000000000000, 0.000000000000000000, 1.000000000000000000 ) ) ;
#4295 = DIRECTION ( 'NONE',  ( -0.6374239897486843054, 0.7705132427757935831, 0.000000000000000000 ) ) ;
#4296 = LINE ( 'NONE', #20356, #441 ) ;
#4297 = ORIENTED_EDGE ( 'NONE', *, *, #11393, .F. ) ;
#4298 = PLANE ( 'NONE',  #2990 ) ;
#4299 = CARTESIAN_POINT ( 'NONE',  ( -3.999999999999996447, 25.61874999877096926, 8.999999999999992895 ) ) ;
#4300 = CARTESIAN_POINT ( 'NONE',  ( 3.756430356249997882, -25.40312499938548285, 11.16877607737301226 ) ) ;
#4302 = ORIENTED_EDGE ( 'NONE', *, *, #14089, .T. ) ;
#4301 = CARTESIAN_POINT ( 'NONE',  ( 3.110308778861319290, 38.49999999999999289, 3.869115154270335477 ) ) ;
#4303 = EDGE_CURVE ( 'NONE', #23296, #14980, #21570, .T. ) ;
#4304 = EDGE_LOOP ( 'NONE', ( #7201, #7831, #1374, #13092 ) ) ;
#4305 = ORIENTED_EDGE ( 'NONE', *, *, #5876, .F. ) ;
#4306 = VERTEX_POINT ( 'NONE', #13218 ) ;
#4307 = CARTESIAN_POINT ( 'NONE',  ( 0.4999838450259764255, -31.09598070739550124, -6.500000000000000000 ) ) ;
#4308 = CARTESIAN_POINT ( 'NONE',  ( -3.756430356249996105, 25.89062499938548356, 6.831223922626973533 ) ) ;
#4309 = VECTOR ( 'NONE', #5742, 1000.000000000000000 ) ;
#4310 = CARTESIAN_POINT ( 'NONE',  ( -1.999999999999998224, 28.90000000000000924, 12.46410161513774639 ) ) ;
#4311 = CARTESIAN_POINT ( 'NONE',  ( 3.756430356250004099, -6.831223922626973533, 0.2906249993854818081 ) ) ;
#4312 = EDGE_CURVE ( 'NONE', #24168, #23712, #19288, .T. ) ;
#4313 = CARTESIAN_POINT ( 'NONE',  ( 3.756430356250004099, 26.97812499938548569, 6.831223922626973533 ) ) ;
#4314 = DIRECTION ( 'NONE',  ( 1.000000000000000000, -0.000000000000000000, -0.000000000000000000 ) ) ;
#4315 = CARTESIAN_POINT ( 'NONE',  ( -1.878215178124995832, 25.74062499938548498, 5.746835883940462963 ) ) ;
#4316 = DIRECTION ( 'NONE',  ( 0.000000000000000000, 0.000000000000000000, -1.000000000000000000 ) ) ;
#4317 = FACE_OUTER_BOUND ( 'NONE', #19471, .T. ) ;
#4318 = DIRECTION ( 'NONE',  ( 0.000000000000000000, 0.000000000000000000, 1.000000000000000000 ) ) ;
#4319 = CARTESIAN_POINT ( 'NONE',  ( -4.000000000000001776, -29.40624999877096357, 11.30940107675849760 ) ) ;
#4320 = DIRECTION ( 'NONE',  ( 0.000000000000000000, -0.000000000000000000, -1.000000000000000000 ) ) ;
#4321 = CARTESIAN_POINT ( 'NONE',  ( -29.09636799667067564, 10.98232076577254368, -6.500000000000000000 ) ) ;
#4322 = CARTESIAN_POINT ( 'NONE',  ( -1.071796769724493448, 29.57634618820329564, 4.999999999999995559 ) ) ;
#4323 = CARTESIAN_POINT ( 'NONE',  ( -3.999999999999997335, 27.96250000000000213, 11.30940107675849404 ) ) ;
#4324 = EDGE_CURVE ( 'NONE', #14942, #12173, #18487, .T. ) ;
#4325 = EDGE_LOOP ( 'NONE', ( #4981, #18199, #3226, #14200 ) ) ;
#4326 = DIRECTION ( 'NONE',  ( 0.000000000000000000, -1.000000000000000000, 0.000000000000000000 ) ) ;
#4328 = EDGE_LOOP ( 'NONE', ( #20005, #25336, #16919, #11886 ) ) ;
#4327 = CARTESIAN_POINT ( 'NONE',  ( -16.16421332384646448, 26.25859848311288403, -6.500000000000000000 ) ) ;
#4329 = ORIENTED_EDGE ( 'NONE', *, *, #170, .T. ) ;
#4330 = VERTEX_POINT ( 'NONE', #17285 ) ;
#4331 = EDGE_LOOP ( 'NONE', ( #13956, #2988, #5146, #1954 ) ) ;
#4332 = ORIENTED_EDGE ( 'NONE', *, *, #16167, .T. ) ;
#4333 = ORIENTED_EDGE ( 'NONE', *, *, #1646, .F. ) ;
#4334 = CARTESIAN_POINT ( 'NONE',  ( 4.000000000000034639, -6.690598923241508622, 2.681249998770965259 ) ) ;
#4335 = EDGE_CURVE ( 'NONE', #3918, #15046, #7065, .T. ) ;
#4336 = ORIENTED_EDGE ( 'NONE', *, *, #10121, .T. ) ;
#4337 = DIRECTION ( 'NONE',  ( -0.000000000000000000, -0.000000000000000000, 1.000000000000000000 ) ) ;
#4338 = CARTESIAN_POINT ( 'NONE',  ( -3.756430356249996994, 27.27812499938548640, 8.999999999999992895 ) ) ;
#4339 = VECTOR ( 'NONE', #1388, 1000.000000000000000 ) ;
#4340 = CARTESIAN_POINT ( 'NONE',  ( 3.756430356250002323, -11.16877607737301226, 3.365624999385485872 ) ) ;
#4341 = CARTESIAN_POINT ( 'NONE',  ( 2.000000000000003553, 25.97500000000000497, 5.535898384862238508 ) ) ;
#4342 = CARTESIAN_POINT ( 'NONE',  ( 17.82786595466764012, 20.48406333262694190, 5.746835883940462963 ) ) ;
#4343 = DIRECTION ( 'NONE',  ( 5.329070518200752183E-15, 0.000000000000000000, 1.000000000000000000 ) ) ;
#4344 = DIRECTION ( 'NONE',  ( 0.000000000000000000, 0.000000000000000000, -1.000000000000000000 ) ) ;
#4345 = CARTESIAN_POINT ( 'NONE',  ( 3.756430356250002323, -11.16877607737301226, 2.353124999385479477 ) ) ;
#4346 = DIRECTION ( 'NONE',  ( -0.000000000000000000, 0.000000000000000000, -1.000000000000000000 ) ) ;
#4347 = CARTESIAN_POINT ( 'NONE',  ( 3.735045420075836212E-15, 29.30312499938548498, 4.662447845253954171 ) ) ;
#4348 = CARTESIAN_POINT ( 'NONE',  ( 2.672651547586948120E-15, -13.33755215474603162, 1.040624999385485472 ) ) ;
#4349 = DIRECTION ( 'NONE',  ( 0.000000000000000000, -0.000000000000000000, 1.000000000000000000 ) ) ;
#4350 = CARTESIAN_POINT ( 'NONE',  ( -1.022599059854450137E-14, 29.16250000000000497, 4.999999999999992006 ) ) ;
#4351 = AXIS2_PLACEMENT_3D ( 'NONE', #10397, #18395, #495 ) ;
#4352 = ORIENTED_EDGE ( 'NONE', *, *, #8233, .T. ) ;
#4353 = ORIENTED_EDGE ( 'NONE', *, *, #22461, .F. ) ;
#4354 = CARTESIAN_POINT ( 'NONE',  ( 3.756430356250002323, 27.91562499938548925, 11.16877607737301226 ) ) ;
#4355 = EDGE_CURVE ( 'NONE', #14319, #1528, #8453, .T. ) ;
#4356 = EDGE_LOOP ( 'NONE', ( #8522, #10203, #9764, #4336 ) ) ;
#4357 = CARTESIAN_POINT ( 'NONE',  ( 3.469446951953614189E-15, -8.999999999999992895, 0.000000000000000000 ) ) ;
#4358 = VERTEX_POINT ( 'NONE', #5118 ) ;
#4359 = CARTESIAN_POINT ( 'NONE',  ( -3.999999999999996447, 28.37500000000000355, 8.999999999999992895 ) ) ;
#4360 = EDGE_CURVE ( 'NONE', #22434, #380, #13096, .T. ) ;
#4361 = ORIENTED_EDGE ( 'NONE', *, *, #24990, .T. ) ;
#4362 = CYLINDRICAL_SURFACE ( 'NONE', #20278, 4.000000000000000000 ) ;
#4363 = ORIENTED_EDGE ( 'NONE', *, *, #16025, .F. ) ;
#4364 = EDGE_CURVE ( 'NONE', #24045, #9259, #1176, .T. ) ;
#4365 = CARTESIAN_POINT ( 'NONE',  ( -21.65113613650310143, 22.32573188046944068, -6.500000000000000000 ) ) ;
#4366 = CARTESIAN_POINT ( 'NONE',  ( 3.756430356250004099, 28.32812499938548356, 6.831223922626973533 ) ) ;
#4367 = DIRECTION ( 'NONE',  ( 1.000000000000000000, 0.000000000000000000, 0.000000000000000000 ) ) ;
#4368 = DIRECTION ( 'NONE',  ( -0.4257792915650782661, -0.9048270524660170233, 0.000000000000000000 ) ) ;
#4369 = CYLINDRICAL_SURFACE ( 'NONE', #11246, 4.000000000000000000 ) ;
#4370 = CARTESIAN_POINT ( 'NONE',  ( 3.918924903856942255, 29.74337361029841276, 9.928636277907717300 ) ) ;
#4371 = B_SPLINE_CURVE_WITH_KNOTS ( 'NONE', 3,
 ( #600, #4111, #14334, #18370, #10639, #2408, #22299, #4374, #12473, #12352 ),
 .UNSPECIFIED., .F., .F.,
 ( 4, 2, 2, 2, 4 ),
 ( 2.789812635309770584E-07, 0.0002324414413947193921, 0.0004646039015259078100, 0.0006967663616570962280, 0.0009289288217882846459 ),
 .UNSPECIFIED. ) ;
#4372 = CARTESIAN_POINT ( 'NONE',  ( 3.756430356250002323, 26.90312499938548640, 11.16877607737301226 ) ) ;
#4373 = PLANE ( 'NONE',  #5511 ) ;
#4374 = CARTESIAN_POINT ( 'NONE',  ( -0.1550712154452952851, 38.97879272568130204, 3.480616423035832518 ) ) ;
#4375 = CARTESIAN_POINT ( 'NONE',  ( -1.999999999999994893, 25.54374999877097352, 5.535898384862237620 ) ) ;
#4376 = FACE_OUTER_BOUND ( 'NONE', #15472, .T. ) ;
#4377 = FACE_OUTER_BOUND ( 'NONE', #4199, .T. ) ;
#4378 = CARTESIAN_POINT ( 'NONE',  ( -0.4995657836784015426, 34.50000000000000000, 3.020833333333324600 ) ) ;
#4379 = ORIENTED_EDGE ( 'NONE', *, *, #809, .T. ) ;
#4380 = CARTESIAN_POINT ( 'NONE',  ( 2.000000000000003997, 28.16874999877096997, 5.535898384862238508 ) ) ;
#4381 = CARTESIAN_POINT ( 'NONE',  ( 20.37029720654250298, 18.85454767869038051, 4.999999999999992895 ) ) ;
#4383 = EDGE_LOOP ( 'NONE', ( #19500, #13715, #698, #5012 ) ) ;
#4382 = CARTESIAN_POINT ( 'NONE',  ( 3.756430356250006319, 27.09062499938548640, 6.831223922626973533 ) ) ;
#4384 = ORIENTED_EDGE ( 'NONE', *, *, #11921, .T. ) ;
#4385 = DIRECTION ( 'NONE',  ( -0.9822872507286872779, 0.1873813145857327056, 0.000000000000000000 ) ) ;
#4386 = CARTESIAN_POINT ( 'NONE',  ( 3.611975211414842679, 38.84312993071436892, 4.645898033752072998 ) ) ;
#4387 = CARTESIAN_POINT ( 'NONE',  ( 3.878215178125003604, -8.999999999999992895, 4.570312499692741781 ) ) ;
#4388 = ORIENTED_EDGE ( 'NONE', *, *, #6750, .T. ) ;
#4389 = ORIENTED_EDGE ( 'NONE', *, *, #10921, .T. ) ;
#4390 = ADVANCED_FACE ( 'NONE', ( #15189 ), #5238, .F. ) ;
#4391 = CARTESIAN_POINT ( 'NONE',  ( -3.756430356250002323, -27.46562499938548640, 11.16877607737301403 ) ) ;
#4392 = CARTESIAN_POINT ( 'NONE',  ( -3.756430356249996105, 27.65312499938548996, 11.16877607737301226 ) ) ;
#4393 = CARTESIAN_POINT ( 'NONE',  ( -2.000000000000000888, -28.91874999877096997, 12.46410161513774817 ) ) ;
#4394 = EDGE_CURVE ( 'NONE', #5166, #22953, #5519, .T. ) ;
#4395 = CARTESIAN_POINT ( 'NONE',  ( 0.000000000000000000, 6.000000000000000000, 19.50000000000000000 ) ) ;
#4396 = ADVANCED_FACE ( 'NONE', ( #15308 ), #13345, .T. ) ;
#4397 = AXIS2_PLACEMENT_3D ( 'NONE', #22487, #16493, #10978 ) ;
#4398 = CARTESIAN_POINT ( 'NONE',  ( -13.24173596767339767, 28.14012133169338270, -6.500000000000000000 ) ) ;
#4399 =( NAMED_UNIT ( * ) PLANE_ANGLE_UNIT ( ) SI_UNIT ( $, .RADIAN. ) );
#4400 =( BOUNDED_CURVE ( )  B_SPLINE_CURVE ( 2, ( #14060, #12086, #9616, #9869, #205, #25573, #3863, #14191, #22161 ),
 .UNSPECIFIED., .F., .F. ) 
 B_SPLINE_CURVE_WITH_KNOTS ( ( 3, 2, 2, 2, 3 ),
 ( 0.7249999999999999778, 0.7333333333333332815, 0.7500000000000000000, 0.7666666666666667185, 0.7750000000000000222 ),
 .UNSPECIFIED. ) 
 CURVE ( )  GEOMETRIC_REPRESENTATION_ITEM ( )  RATIONAL_B_SPLINE_CURVE ( ( 0.9330127018922194093, 0.9330127018922194093, 1.000000000000000000, 0.8660254037844387076, 1.000000000000000000, 0.8660254037844387076, 1.000000000000000000, 0.9330127018922194093, 0.9330127018922194093 ) ) 
 REPRESENTATION_ITEM ( '' )  );
#4401 = CARTESIAN_POINT ( 'NONE',  ( -18.28012134629558716, 25.16042852506110705, -6.500000000000000000 ) ) ;
#4402 = CARTESIAN_POINT ( 'NONE',  ( 14.54246377227340048, -27.49048467073863833, -2.750000000000000000 ) ) ;
#4403 = CYLINDRICAL_SURFACE ( 'NONE', #8424, 4.000000000000000000 ) ;
#4404 = CARTESIAN_POINT ( 'NONE',  ( 19.87733689425031613, 21.39308642210229294, 4.999999999999995559 ) ) ;
#4405 = CARTESIAN_POINT ( 'NONE',  ( 18.25213002337956780, 20.90832740133887313, 12.25316411605951927 ) ) ;
#4406 = CARTESIAN_POINT ( 'NONE',  ( 23.03842281366518208, 17.38156856417272067, 6.690598923241489970 ) ) ;
#4407 = ORIENTED_EDGE ( 'NONE', *, *, #11890, .F. ) ;
#4408 = CARTESIAN_POINT ( 'NONE',  ( 0.000000000000000000, 0.000000000000000000, -6.500000000000000000 ) ) ;
#4409 = FACE_OUTER_BOUND ( 'NONE', #21758, .T. ) ;
#4410 =( BOUNDED_CURVE ( )  B_SPLINE_CURVE ( 2, ( #18135, #1913, #18246, #9873, #14195, #11840, #25829, #23614, #5820 ),
 .UNSPECIFIED., .F., .F. ) 
 B_SPLINE_CURVE_WITH_KNOTS ( ( 3, 2, 2, 2, 3 ),
 ( 0.6750000000000000444, 0.6833333333333333481, 0.6999999999999999556, 0.7166666666666666741, 0.7249999999999999778 ),
 .UNSPECIFIED. ) 
 CURVE ( )  GEOMETRIC_REPRESENTATION_ITEM ( )  RATIONAL_B_SPLINE_CURVE ( ( 0.9330127018922194093, 0.9330127018922198534, 1.000000000000000000, 0.8660254037844387076, 1.000000000000000000, 0.8660254037844387076, 1.000000000000000000, 0.9330127018922194093, 0.9330127018922194093 ) ) 
 REPRESENTATION_ITEM ( '' )  );
#4411 = CARTESIAN_POINT ( 'NONE',  ( -3.756430356249997882, 25.85312499938548925, 11.16877607737301226 ) ) ;
#4413 = ORIENTED_EDGE ( 'NONE', *, *, #12834, .F. ) ;
#4412 = CARTESIAN_POINT ( 'NONE',  ( -3.974466138550253103, 29.73560671006806899, 8.477544402765669673 ) ) ;
#4414 = CARTESIAN_POINT ( 'NONE',  ( 0.000000000000000000, 0.000000000000000000, 20.00000000000000000 ) ) ;
#4415 = CARTESIAN_POINT ( 'NONE',  ( 4.000000000000032863, -11.30940107675847983, 1.312499999999998890 ) ) ;
#4416 = VERTEX_POINT ( 'NONE', #15955 ) ;
#4417 = CARTESIAN_POINT ( 'NONE',  ( 0.000000000000000000, 0.000000000000000000, 0.000000000000000000 ) ) ;
#4418 = DIRECTION ( 'NONE',  ( 0.000000000000000000, 0.000000000000000000, 1.000000000000000000 ) ) ;
#4419 = CARTESIAN_POINT ( 'NONE',  ( -3.735045420075836212E-15, -26.15312499938548285, 4.662447845253954171 ) ) ;
#4421 = EDGE_LOOP ( 'NONE', ( #18563, #3431, #15528, #4190 ) ) ;
#4420 = CARTESIAN_POINT ( 'NONE',  ( 31.06601413805602263, -1.453535542772716793, -6.500000000000000000 ) ) ;
#4422 = VERTEX_POINT ( 'NONE', #13860 ) ;
#4423 = EDGE_CURVE ( 'NONE', #15106, #7204, #1955, .T. ) ;
#4424 = CARTESIAN_POINT ( 'NONE',  ( -3.756430356250004099, -25.62812499938548072, 6.831223922626973533 ) ) ;
#4425 = ORIENTED_EDGE ( 'NONE', *, *, #25507, .F. ) ;
#4426 = PRODUCT ( 'glass', 'glass', '', ( #9094 ) ) ;
#4427 = ORIENTED_EDGE ( 'NONE', *, *, #9829, .F. ) ;
#4428 = SURFACE_STYLE_FILL_AREA ( #18679 ) ;
#4429 = CARTESIAN_POINT ( 'NONE',  ( -1.999999999999998224, 27.04374999877096641, 12.46410161513774639 ) ) ;
#4430 = EDGE_CURVE ( 'NONE', #25396, #19442, #11352, .T. ) ;
#4431 = CARTESIAN_POINT ( 'NONE',  ( 3.752267015613588906E-15, -4.381197846482986158, 1.912500000000001865 ) ) ;
#4432 = CARTESIAN_POINT ( 'NONE',  ( 3.756430356250004099, -6.831223922626973533, 1.640624999385484895 ) ) ;
#4433 = CARTESIAN_POINT ( 'NONE',  ( 3.756430356250002323, 29.71562499938548640, 11.16877607737301226 ) ) ;
#4434 = EDGE_CURVE ( 'NONE', #19279, #184, #6767, .T. ) ;
#4435 = CARTESIAN_POINT ( 'NONE',  ( 3.469446951953614189E-15, 35.50000000000000711, 4.999999999999992006 ) ) ;
#4436 = DIRECTION ( 'NONE',  ( 0.000000000000000000, 0.000000000000000000, 1.000000000000000000 ) ) ;
#4437 = CARTESIAN_POINT ( 'NONE',  ( 3.756430356250003211, 26.97812499938547859, 6.831223922626973533 ) ) ;
#4438 = DIRECTION ( 'NONE',  ( 0.6374239897486995154, 0.7705132427757811486, 0.000000000000000000 ) ) ;
#4439 = DIRECTION ( 'NONE',  ( 0.000000000000000000, 0.000000000000000000, 1.000000000000000000 ) ) ;
#4440 = CARTESIAN_POINT ( 'NONE',  ( -1.999999999999995781, -5.535898384862237620, 0.9937499987709673688 ) ) ;
#4441 = CARTESIAN_POINT ( 'NONE',  ( -4.000000000000003553, -28.54374999877096997, 8.999999999999992895 ) ) ;
#4442 = CARTESIAN_POINT ( 'NONE',  ( -4.000000000000000000, 27.47500000000000142, 8.999999999999992895 ) ) ;
#4443 = CARTESIAN_POINT ( 'NONE',  ( 0.000000000000000000, 0.000000000000000000, 1.000000000000000000 ) ) ;
#4444 = CARTESIAN_POINT ( 'NONE',  ( 3.999999999999997335, -25.26249999999999929, 11.30940107675849404 ) ) ;
#4445 = ADVANCED_BREP_SHAPE_REPRESENTATION ( '', ( #5394, #21036 ), #21481 ) ;
#4446 = CARTESIAN_POINT ( 'NONE',  ( -3.469446951953614189E-15, -30.00000000000000355, 4.999999999999992006 ) ) ;
#4447 = ORIENTED_EDGE ( 'NONE', *, *, #10150, .T. ) ;
#4448 = CARTESIAN_POINT ( 'NONE',  ( 0.000000000000000000, 0.000000000000000000, -6.500000000000000000 ) ) ;
#4450 = ORIENTED_EDGE ( 'NONE', *, *, #24313, .T. ) ;
#4449 = CARTESIAN_POINT ( 'NONE',  ( -3.878215178125003604, -29.57031249969274356, 8.999999999999992895 ) ) ;
#4451 = ORIENTED_EDGE ( 'NONE', *, *, #5993, .F. ) ;
#4452 = ORIENTED_EDGE ( 'NONE', *, *, #3456, .T. ) ;
#4453 = ORIENTED_EDGE ( 'NONE', *, *, #25200, .F. ) ;
#4454 = ORIENTED_EDGE ( 'NONE', *, *, #24551, .T. ) ;
#4455 = VERTEX_POINT ( 'NONE', #22220 ) ;
#4456 = CARTESIAN_POINT ( 'NONE',  ( -1.071796769724494558, -27.79240381056766651, 4.999999999999992895 ) ) ;
#4457 = ORIENTED_EDGE ( 'NONE', *, *, #9338, .F. ) ;
#4458 = CYLINDRICAL_SURFACE ( 'NONE', #23872, 0.5000000000000004441 ) ;
#4459 = CARTESIAN_POINT ( 'NONE',  ( 3.756430356250002323, 25.66562499938548569, 11.16877607737301403 ) ) ;
#4460 = ADVANCED_FACE ( 'NONE', ( #16084 ), #12279, .T. ) ;
#4461 = CARTESIAN_POINT ( 'NONE',  ( 1.878215178125004048, -5.746835883940462963, 1.678124999385483651 ) ) ;
#4462 = SURFACE_STYLE_FILL_AREA ( #16904 ) ;
#4463 = CARTESIAN_POINT ( 'NONE',  ( 18.97034911358585418, 18.97034911358578668, 13.33755215474602984 ) ) ;
#4464 = CARTESIAN_POINT ( 'NONE',  ( 0.000000000000000000, 0.000000000000000000, -6.500000000000000000 ) ) ;
#4465 = FACE_OUTER_BOUND ( 'NONE', #1443, .T. ) ;
#4466 = CARTESIAN_POINT ( 'NONE',  ( -1.878215178124998497, -12.25316411605951927, 2.690624999385483385 ) ) ;
#4467 = SURFACE_STYLE_FILL_AREA ( #19923 ) ;
#4468 = CARTESIAN_POINT ( 'NONE',  ( 2.620986760973688460E-15, -13.61880215351699874, 3.937499999999998224 ) ) ;
#4469 = DIRECTION ( 'NONE',  ( 0.000000000000000000, -0.000000000000000000, 1.000000000000000000 ) ) ;
#4470 = DIRECTION ( 'NONE',  ( -0.000000000000000000, -0.000000000000000000, 1.000000000000000000 ) ) ;
#4471 = CARTESIAN_POINT ( 'NONE',  ( 3.756430356250002323, -11.16877607737301403, 1.565624999385483163 ) ) ;
#4472 = CARTESIAN_POINT ( 'NONE',  ( 1.071796769724494558, 25.99240381056766580, 4.999999999999992895 ) ) ;
#4473 = DIRECTION ( 'NONE',  ( 0.000000000000000000, 0.000000000000000000, 1.000000000000000000 ) ) ;
#4474 = EDGE_LOOP ( 'NONE', ( #12143, #4163, #21216, #18232 ) ) ;
#4475 = VERTEX_POINT ( 'NONE', #261 ) ;
#4476 = CARTESIAN_POINT ( 'NONE',  ( 3.756430356250002323, 27.46562499938548640, 11.16877607737301226 ) ) ;
#4477 = VERTEX_POINT ( 'NONE', #4307 ) ;
#4478 = DIRECTION ( 'NONE',  ( 1.000000000000000000, 0.000000000000000000, 0.000000000000000000 ) ) ;
#4479 = VERTEX_POINT ( 'NONE', #19857 ) ;
#4480 = CARTESIAN_POINT ( 'NONE',  ( -12.78762572734029312, 28.34936733434213352, 1.000000000000000000 ) ) ;
#4481 = EDGE_LOOP ( 'NONE', ( #6289, #22861, #1024, #11460 ) ) ;
#4482 = CARTESIAN_POINT ( 'NONE',  ( 0.000000000000000000, 0.000000000000000000, 1.000000000000000000 ) ) ;
#4483 = SHAPE_REPRESENTATION ( 'indicator hand', ( #21036 ), #24374 ) ;
#4484 = CARTESIAN_POINT ( 'NONE',  ( -3.469446951953614189E-15, -30.00000000000000355, 8.999999999999992895 ) ) ;
#4485 = ORIENTED_EDGE ( 'NONE', *, *, #20590, .F. ) ;
#4486 = LINE ( 'NONE', #14704, #7644 ) ;
#4487 = CARTESIAN_POINT ( 'NONE',  ( 3.756430356250002323, 26.00312499938548427, 11.16877607737301226 ) ) ;
#4488 = DIRECTION ( 'NONE',  ( 1.000000000000000000, 0.000000000000000000, 0.000000000000000000 ) ) ;
#4489 = EDGE_CURVE ( 'NONE', #10075, #2553, #14309, .T. ) ;
#4490 = PLANE ( 'NONE',  #9233 ) ;
#4491 = CARTESIAN_POINT ( 'NONE',  ( -3.137519842735244810E-15, 26.91249999999999787, 4.999999999999991118 ) ) ;
#4492 = CARTESIAN_POINT ( 'NONE',  ( 4.000000000000003553, 29.73213749463701561, 8.999999999999992895 ) ) ;
#4493 = EDGE_CURVE ( 'NONE', #14796, #17688, #20148, .T. ) ;
#4494 = CARTESIAN_POINT ( 'NONE',  ( 3.735045420075836212E-15, 27.50312499938548783, 4.662447845253954171 ) ) ;
#4495 = EDGE_CURVE ( 'NONE', #22067, #5321, #19742, .T. ) ;
#4496 = DIRECTION ( 'NONE',  ( 0.7705132427757999114, 0.6374239897486768669, 0.000000000000000000 ) ) ;
#4497 = CARTESIAN_POINT ( 'NONE',  ( 23.36987911821542951, 17.71302486872297166, 8.999999999999992895 ) ) ;
#4498 = EDGE_CURVE ( 'NONE', #25487, #7861, #8043, .T. ) ;
#4499 = CARTESIAN_POINT ( 'NONE',  ( 4.000000000000003553, 25.39374999877097494, 8.999999999999992895 ) ) ;
#4500 = CARTESIAN_POINT ( 'NONE',  ( -1.999999999999995781, 29.14374999877096784, 5.535898384862237620 ) ) ;
#4501 = DIRECTION ( 'NONE',  ( 1.000000000000000000, 0.000000000000000000, 0.000000000000000000 ) ) ;
#4502 = CARTESIAN_POINT ( 'NONE',  ( 5.532151103383248447, 38.49999999999999289, 11.32277940608563149 ) ) ;
#4503 = ORIENTED_EDGE ( 'NONE', *, *, #20547, .T. ) ;
#4504 = CARTESIAN_POINT ( 'NONE',  ( -3.999999999999997335, 29.25624999877096499, 11.30940107675849404 ) ) ;
#4505 = CARTESIAN_POINT ( 'NONE',  ( -2.000000000000000888, -28.07500000000000284, 12.46410161513774817 ) ) ;
#4507 = VERTEX_POINT ( 'NONE', #17661 ) ;
#4506 = CARTESIAN_POINT ( 'NONE',  ( -3.756430356249997882, 28.66562499938548925, 11.16877607737301048 ) ) ;
#4508 = VERTEX_POINT ( 'NONE', #20120 ) ;
#4509 = CARTESIAN_POINT ( 'NONE',  ( -3.999999999999995559, 28.73124999877096997, 6.690598923241487306 ) ) ;
#4510 = FACE_OUTER_BOUND ( 'NONE', #13924, .T. ) ;
#4511 = CARTESIAN_POINT ( 'NONE',  ( -1.071796769724487230, 25.71115380933864003, 12.99999999999999467 ) ) ;
#4512 = ORIENTED_EDGE ( 'NONE', *, *, #22869, .T. ) ;
#4513 = ORIENTED_EDGE ( 'NONE', *, *, #21124, .F. ) ;
#4514 = CARTESIAN_POINT ( 'NONE',  ( 1.878215178124998497, -27.80312499938548498, 12.25316411605951927 ) ) ;
#4515 = CARTESIAN_POINT ( 'NONE',  ( 6.009258394948636914E-15, 27.50312499938549138, 4.662447845253954171 ) ) ;
#4516 = CARTESIAN_POINT ( 'NONE',  ( 25.16042852506077665, -18.28012134629603835, 1.000000000000000000 ) ) ;
#4517 = CARTESIAN_POINT ( 'NONE',  ( 4.000000000000000888, 26.31250000000000711, 11.30940107675849760 ) ) ;
#4518 = VECTOR ( 'NONE', #6281, 1000.000000000000000 ) ;
#4519 = CARTESIAN_POINT ( 'NONE',  ( 2.000000000000003997, -5.535898384862238508, 0.9750000000000001998 ) ) ;
#4520 = AXIS2_PLACEMENT_3D ( 'NONE', #21780, #4110, #1784 ) ;
#4521 = CARTESIAN_POINT ( 'NONE',  ( 0.000000000000000000, 0.000000000000000000, 0.000000000000000000 ) ) ;
#4522 = EDGE_CURVE ( 'NONE', #10325, #674, #7832, .T. ) ;
#4523 = CARTESIAN_POINT ( 'NONE',  ( 3.756430356250003655, -8.999999999999992895, 0.1406249993854830072 ) ) ;
#4524 = CIRCLE ( 'NONE', #22913, 0.5000000000000005551 ) ;
#4525 = DIRECTION ( 'NONE',  ( 1.000000000000000000, 0.000000000000000000, 0.000000000000000000 ) ) ;
#4526 = CARTESIAN_POINT ( 'NONE',  ( -10.08469938919458286, 29.41953157733104263, -6.500000000000000000 ) ) ;
#4527 = CARTESIAN_POINT ( 'NONE',  ( 4.000000000000003553, 25.44999999999999929, 8.999999999999992895 ) ) ;
#4528 = CARTESIAN_POINT ( 'NONE',  ( 21.09621640565530853, 15.78382164973649537, 6.831223922626973533 ) ) ;
#4529 = CARTESIAN_POINT ( 'NONE',  ( 17.80583263288473717, 23.46268688237704225, 6.690598923241487306 ) ) ;
#4530 = EDGE_CURVE ( 'NONE', #4728, #15879, #22667, .T. ) ;
#4531 = DIRECTION ( 'NONE',  ( 0.000000000000000000, 0.000000000000000000, 1.000000000000000000 ) ) ;
#4532 = CARTESIAN_POINT ( 'NONE',  ( 24.00000000000000355, 0.000000000000000000, 19.00000000000000000 ) ) ;
#4533 = CARTESIAN_POINT ( 'NONE',  ( 3.756430356250004099, 26.52812499938548285, 6.831223922626973533 ) ) ;
#4534 = ADVANCED_FACE ( 'NONE', ( #12305 ), #16201, .T. ) ;
#4536 = ORIENTED_EDGE ( 'NONE', *, *, #5627, .T. ) ;
#4535 = DIRECTION ( 'NONE',  ( 0.000000000000000000, -0.000000000000000000, 1.000000000000000000 ) ) ;
#4537 = CARTESIAN_POINT ( 'NONE',  ( -3.999999999999996447, 25.58124999877097139, 6.690598923241487306 ) ) ;
#4538 = DIRECTION ( 'NONE',  ( -0.000000000000000000, 0.000000000000000000, 1.000000000000000000 ) ) ;
#4539 = ORIENTED_EDGE ( 'NONE', *, *, #15626, .F. ) ;
#4540 = CARTESIAN_POINT ( 'NONE',  ( -1.071796769724488563, 28.91740381056766651, 12.99999999999999289 ) ) ;
#4541 = DIRECTION ( 'NONE',  ( 0.000000000000000000, 0.000000000000000000, 1.000000000000000000 ) ) ;
#4542 = CARTESIAN_POINT ( 'NONE',  ( -2.672651547586948120E-15, -26.82812499938548356, 13.33755215474602984 ) ) ;
#4544 = VERTEX_POINT ( 'NONE', #21836 ) ;
#4543 = CARTESIAN_POINT ( 'NONE',  ( 15.61822102945791002, 21.27507527895022221, 6.690598923241487306 ) ) ;
#4545 = DIRECTION ( 'NONE',  ( 0.000000000000000000, 0.000000000000000000, 1.000000000000000000 ) ) ;
#4546 = ORIENTED_EDGE ( 'NONE', *, *, #1319, .F. ) ;
#4547 = CARTESIAN_POINT ( 'NONE',  ( 3.756430356249995661, -26.67812499938548498, 6.831223922626973533 ) ) ;
#4548 = ORIENTED_EDGE ( 'NONE', *, *, #17695, .T. ) ;
#4549 = CIRCLE ( 'NONE', #10755, 0.4999999999999999445 ) ;
#4550 = ORIENTED_EDGE ( 'NONE', *, *, #23479, .T. ) ;
#4551 =( NAMED_UNIT ( * ) SI_UNIT ( $, .STERADIAN. ) SOLID_ANGLE_UNIT ( ) );
#4552 = CARTESIAN_POINT ( 'NONE',  ( 1.878215178125001605, 26.07812499938549067, 12.25316411605952283 ) ) ;
#4553 = AXIS2_PLACEMENT_3D ( 'NONE', #22455, #18552, #12517 ) ;
#4554 = DIRECTION ( 'NONE',  ( 0.000000000000000000, 0.000000000000000000, 1.000000000000000000 ) ) ;
#4555 =( BOUNDED_CURVE ( )  B_SPLINE_CURVE ( 2, ( #2450, #8721, #22852, #4537, #633, #884, #10553, #8868, #12266 ),
 .UNSPECIFIED., .F., .F. ) 
 B_SPLINE_CURVE_WITH_KNOTS ( ( 3, 2, 2, 2, 3 ),
 ( 0.02500000000000000486, 0.03333333333333333287, 0.05000000000000000278, 0.06666666666666666574, 0.07500000000000001110 ),
 .UNSPECIFIED. ) 
 CURVE ( )  GEOMETRIC_REPRESENTATION_ITEM ( )  RATIONAL_B_SPLINE_CURVE ( ( 0.9330127018922194093, 0.9330127018922194093, 1.000000000000000000, 0.8660254037844387076, 1.000000000000000000, 0.8660254037844387076, 1.000000000000000000, 0.9330127018922191873, 0.9330127018922192983 ) ) 
 REPRESENTATION_ITEM ( '' )  );
#4556 = CARTESIAN_POINT ( 'NONE',  ( 1.878215178125000939, -12.25316411605952283, 1.528124999385482852 ) ) ;
#4557 = CARTESIAN_POINT ( 'NONE',  ( 22.49925389301043666, 19.67082676826417398, 12.46410161513774817 ) ) ;
#4558 =( BOUNDED_CURVE ( )  B_SPLINE_CURVE ( 2, ( #16190, #24427, #18666, #6504, #22456, #12518, #2592, #10554, #18553 ),
 .UNSPECIFIED., .F., .F. ) 
 B_SPLINE_CURVE_WITH_KNOTS ( ( 3, 2, 2, 2, 3 ),
 ( 0.3750000000000000000, 0.3833333333333333592, 0.4000000000000000222, 0.4166666666666666852, 0.4250000000000000444 ),
 .UNSPECIFIED. ) 
 CURVE ( )  GEOMETRIC_REPRESENTATION_ITEM ( )  RATIONAL_B_SPLINE_CURVE ( ( 0.9330127018922194093, 0.9330127018922194093, 1.000000000000000000, 0.8660254037844387076, 1.000000000000000000, 0.8660254037844387076, 1.000000000000000000, 0.9330127018922191873, 0.9330127018922194093 ) ) 
 REPRESENTATION_ITEM ( '' )  );
#4559 = CARTESIAN_POINT ( 'NONE',  ( -3.756430356249995661, 25.77812499938548640, 6.831223922626973533 ) ) ;
#4560 = CARTESIAN_POINT ( 'NONE',  ( -28.41604871112473418, -11.44867358849319849, -6.500000000000000000 ) ) ;
#4561 = AXIS2_PLACEMENT_3D ( 'NONE', #17278, #7825, #3913 ) ;
#4562 = CARTESIAN_POINT ( 'NONE',  ( -3.999999999999980904, -6.690598923241480200, 3.787499999999999201 ) ) ;
#4563 = EDGE_CURVE ( 'NONE', #5989, #20109, #6261, .T. ) ;
#4564 = CARTESIAN_POINT ( 'NONE',  ( 1.878215178125004048, 26.11562499938548498, 5.746835883940462963 ) ) ;
#4565 = DIRECTION ( 'NONE',  ( -0.7071067811865487940, -0.7071067811865463515, 0.000000000000000000 ) ) ;
#4566 = CARTESIAN_POINT ( 'NONE',  ( 0.000000000000000000, 0.000000000000000000, -6.500000000000000000 ) ) ;
#4567 = CARTESIAN_POINT ( 'NONE',  ( 4.000000000000030198, -6.690598923241506846, 0.8812499987709628835 ) ) ;
#4568 = CARTESIAN_POINT ( 'NONE',  ( -1.878215178125004048, -25.77812499938548640, 5.746835883940462963 ) ) ;
#4569 = CARTESIAN_POINT ( 'NONE',  ( 3.756430356250004099, 29.34062499938548640, 6.831223922626973533 ) ) ;
#4571 = ADVANCED_FACE ( 'NONE', ( #21698 ), #19740, .F. ) ;
#4570 = VECTOR ( 'NONE', #1220, 1000.000000000000000 ) ;
#4572 = CARTESIAN_POINT ( 'NONE',  ( -0.7500000000000000000, 0.000000000000000000, 18.19999999999999929 ) ) ;
#4574 = DIRECTION ( 'NONE',  ( 0.000000000000000000, -0.000000000000000000, -1.000000000000000000 ) ) ;
#4573 = AXIS2_PLACEMENT_3D ( 'NONE', #19906, #13651, #23980 ) ;
#4575 = CARTESIAN_POINT ( 'NONE',  ( 1.774938052278379752, -29.94842879300231075, 5.405792698933810314 ) ) ;
#4576 = ORIENTED_EDGE ( 'NONE', *, *, #5304, .F. ) ;
#4577 = CARTESIAN_POINT ( 'NONE',  ( 3.469446951953614189E-15, 39.50000000000000000, 8.999999999999992895 ) ) ;
#4579 = VERTEX_POINT ( 'NONE', #25749 ) ;
#4578 = LINE ( 'NONE', #4327, #13329 ) ;
#4580 = EDGE_LOOP ( 'NONE', ( #3878, #13681, #18935, #1565 ) ) ;
#4581 = CIRCLE ( 'NONE', #3947, 31.10000000000000142 ) ;
#4582 = VERTEX_POINT ( 'NONE', #15817 ) ;
#4583 = VERTEX_POINT ( 'NONE', #23786 ) ;
#4584 = ORIENTED_EDGE ( 'NONE', *, *, #19209, .F. ) ;
#4585 = EDGE_LOOP ( 'NONE', ( #10350, #12454, #16439, #4083 ) ) ;
#4586 = CARTESIAN_POINT ( 'NONE',  ( 3.469446951953614189E-15, 30.00000000000000355, 8.999999999999992895 ) ) ;
#4587 = CIRCLE ( 'NONE', #1245, 0.7500000000000001110 ) ;
#4588 = CIRCLE ( 'NONE', #1, 0.5000000000000002220 ) ;
#4589 = ORIENTED_EDGE ( 'NONE', *, *, #6278, .F. ) ;
#4590 = DIRECTION ( 'NONE',  ( -0.000000000000000000, 0.000000000000000000, 1.000000000000000000 ) ) ;
#4591 = CARTESIAN_POINT ( 'NONE',  ( 3.756430356250002323, 27.91562499938548569, 11.16877607737301403 ) ) ;
#4592 = CIRCLE ( 'NONE', #1249, 1.000000000000000000 ) ;
#4593 = CARTESIAN_POINT ( 'NONE',  ( -1.878215178124995832, -5.746835883940462963, 2.653124999385483740 ) ) ;
#4594 = DIRECTION ( 'NONE',  ( -0.000000000000000000, -1.000000000000000000, -0.000000000000000000 ) ) ;
#4595 = CARTESIAN_POINT ( 'NONE',  ( 15.62472262396960154, 20.93711737988828503, 11.16877607737301226 ) ) ;
#4596 = CARTESIAN_POINT ( 'NONE',  ( -25.83240171513484285, -3.403349963601435935, 20.00001200000000168 ) ) ;
#4597 = CIRCLE ( 'NONE', #16727, 6.000000000000000000 ) ;
#4598 = CARTESIAN_POINT ( 'NONE',  ( -3.756430356249995661, -6.831223922626973533, 2.578124999385481342 ) ) ;
#4599 = CARTESIAN_POINT ( 'NONE',  ( -19.43607991389006528, -24.27856662945486832, 1.000000000000000000 ) ) ;
#4600 = CARTESIAN_POINT ( 'NONE',  ( 4.000000000000001776, -11.30940107675849760, 3.562499999999996891 ) ) ;
#4601 = DIRECTION ( 'NONE',  ( 0.000000000000000000, 1.000000000000000000, 0.000000000000000000 ) ) ;
#4602 = ADVANCED_FACE ( 'NONE', ( #5874 ), #13989, .T. ) ;
#4603 = CARTESIAN_POINT ( 'NONE',  ( 0.000000000000000000, 0.000000000000000000, -6.500000000000000000 ) ) ;
#4604 = CIRCLE ( 'NONE', #7941, 31.10000000000000142 ) ;
#4605 = CARTESIAN_POINT ( 'NONE',  ( -3.756430356249997438, -11.16877607737301048, 0.9656249993854834068 ) ) ;
#4606 = AXIS2_PLACEMENT_3D ( 'NONE', #23191, #25164, #9339 ) ;
#4607 = CARTESIAN_POINT ( 'NONE',  ( 4.000000000000003553, 27.68124999877096926, 6.690598923241489970 ) ) ;
#4608 = ORIENTED_EDGE ( 'NONE', *, *, #21958, .T. ) ;
#4609 = VERTEX_POINT ( 'NONE', #8493 ) ;
#4610 = CARTESIAN_POINT ( 'NONE',  ( -3.756430356249997882, 27.72812499938548569, 8.999999999999992895 ) ) ;
#4611 = CIRCLE ( 'NONE', #2522, 0.5000000000000001110 ) ;
#4612 = EDGE_CURVE ( 'NONE', #3077, #15986, #23092, .T. ) ;
#4613 = VERTEX_POINT ( 'NONE', #8616 ) ;
#4614 = LINE ( 'NONE', #24373, #7874 ) ;
#4615 = ORIENTED_EDGE ( 'NONE', *, *, #25156, .F. ) ;
#4616 = CARTESIAN_POINT ( 'NONE',  ( -1.999999999999995781, 26.05000000000000071, 5.535898384862237620 ) ) ;
#4617 = EDGE_LOOP ( 'NONE', ( #12667, #23957, #3433, #6003 ) ) ;
#4618 = FACE_OUTER_BOUND ( 'NONE', #10624, .T. ) ;
#4619 = ADVANCED_FACE ( 'NONE', ( #16866 ), #16343, .F. ) ;
#4620 = CIRCLE ( 'NONE', #20927, 31.10000000000000142 ) ;
#4621 = ORIENTED_EDGE ( 'NONE', *, *, #8841, .T. ) ;
#4622 = DIRECTION ( 'NONE',  ( 0.000000000000000000, 1.000000000000000000, -0.000000000000000000 ) ) ;
#4623 = CARTESIAN_POINT ( 'NONE',  ( 1.878215178125000939, 29.56562499938548427, 12.25316411605952283 ) ) ;
#4624 = CARTESIAN_POINT ( 'NONE',  ( 19.03001124868299243, 19.03001124868293559, 4.999999999999991118 ) ) ;
#4625 = AXIS2_PLACEMENT_3D ( 'NONE', #8627, #14645, #17125 ) ;
#4626 = AXIS2_PLACEMENT_3D ( 'NONE', #564, #24598, #2261 ) ;
#4627 = MANIFOLD_SOLID_BREP ( 'CirPattern1', #5043 ) ;
#4628 = DIRECTION ( 'NONE',  ( -0.000000000000000000, -0.000000000000000000, -1.000000000000000000 ) ) ;
#4629 = CARTESIAN_POINT ( 'NONE',  ( -3.999999999999996447, 26.53750000000000497, 6.690598923241487306 ) ) ;
#4630 = CARTESIAN_POINT ( 'NONE',  ( -1.999999999999996669, 29.35000000000000853, 12.46410161513774639 ) ) ;
#4631 = CIRCLE ( 'NONE', #13411, 0.4999999999999998890 ) ;
#4632 = AXIS2_PLACEMENT_3D ( 'NONE', #23250, #5093, #9512 ) ;
#4633 = CARTESIAN_POINT ( 'NONE',  ( -1.878215178124998497, 28.59062499938548285, 12.25316411605951927 ) ) ;
#4634 = DIRECTION ( 'NONE',  ( 1.000000000000000000, 0.000000000000000000, 0.000000000000000000 ) ) ;
#4635 = AXIS2_PLACEMENT_3D ( 'NONE', #3983, #2158, #13661 ) ;
#4636 = CARTESIAN_POINT ( 'NONE',  ( 17.58044234725058175, 23.23729659674288683, 11.30940107675849404 ) ) ;
#4637 = PRODUCT_DEFINITION_SHAPE ( 'NONE', 'NONE',  #25880 ) ;
#4638 = CYLINDRICAL_SURFACE ( 'NONE', #491, 0.5000000000000004441 ) ;
#4639 = CYLINDRICAL_SURFACE ( 'NONE', #3859, 26.00000000000000355 ) ;
#4640 = AXIS2_PLACEMENT_3D ( 'NONE', #3346, #19543, #13431 ) ;
#4641 = CARTESIAN_POINT ( 'NONE',  ( -3.756430356250003655, -27.39062499938548356, 8.999999999999992895 ) ) ;
#4642 = CIRCLE ( 'NONE', #21764, 0.5000000000000003331 ) ;
#4643 = ADVANCED_FACE ( 'NONE', ( #24697 ), #8882, .F. ) ;
#4644 = CARTESIAN_POINT ( 'NONE',  ( 5.201400854508229088, 38.97868814324866094, 10.85315172130059480 ) ) ;
#4645 = ORIENTED_EDGE ( 'NONE', *, *, #23598, .T. ) ;
#4646 = CARTESIAN_POINT ( 'NONE',  ( -3.999999999999996447, 29.66874999877096997, 8.999999999999992895 ) ) ;
#4647 = CARTESIAN_POINT ( 'NONE',  ( 1.999999999999998224, -29.35000000000000142, 12.46410161513774639 ) ) ;
#4649 = VERTEX_POINT ( 'NONE', #2726 ) ;
#4648 = CARTESIAN_POINT ( 'NONE',  ( 3.756430356250004987, 29.75312499938549138, 8.999999999999992895 ) ) ;
#4650 = VERTEX_POINT ( 'NONE', #12676 ) ;
#4651 = DIRECTION ( 'NONE',  ( -0.000000000000000000, -1.000000000000000000, -0.000000000000000000 ) ) ;
#4652 = EDGE_CURVE ( 'NONE', #22312, #6939, #25182, .T. ) ;
#4653 = DIRECTION ( 'NONE',  ( 0.000000000000000000, 0.000000000000000000, 1.000000000000000000 ) ) ;
#4654 = ORIENTED_EDGE ( 'NONE', *, *, #5596, .F. ) ;
#4655 = CARTESIAN_POINT ( 'NONE',  ( -3.756430356250003211, -27.99062499938548498, 6.831223922626973533 ) ) ;
#4656 = CARTESIAN_POINT ( 'NONE',  ( 3.756430356250006319, 28.77812499938548640, 6.831223922626973533 ) ) ;
#4657 = CARTESIAN_POINT ( 'NONE',  ( 19.92142043288880160, 18.40567090503668979, 12.99999999999999467 ) ) ;
#4658 = CIRCLE ( 'NONE', #21797, 0.5000000000000003331 ) ;
#4659 = DIRECTION ( 'NONE',  ( 0.000000000000000000, 0.000000000000000000, 1.000000000000000000 ) ) ;
#4660 = CARTESIAN_POINT ( 'NONE',  ( -3.756430356249996549, 26.71562499938548996, 8.999999999999992895 ) ) ;
#4661 = CIRCLE ( 'NONE', #19271, 0.5000000000000003331 ) ;
#4662 = VECTOR ( 'NONE', #4469, 1000.000000000000000 ) ;
#4663 = DIRECTION ( 'NONE',  ( 0.000000000000000000, -1.000000000000000000, 0.000000000000000000 ) ) ;
#4664 = DIRECTION ( 'NONE',  ( 0.000000000000000000, 0.000000000000000000, 1.000000000000000000 ) ) ;
#4665 = CIRCLE ( 'NONE', #25298, 0.4999999999999999445 ) ;
#4666 = FACE_OUTER_BOUND ( 'NONE', #3618, .T. ) ;
#4667 = CIRCLE ( 'NONE', #9268, 4.000000000000000000 ) ;
#4668 = CARTESIAN_POINT ( 'NONE',  ( 23.65168074169088186, 18.16705623898524280, 8.999999999999992895 ) ) ;
#4669 = CARTESIAN_POINT ( 'NONE',  ( 16.58607343533794065, 22.24292768483024574, 11.30940107675849404 ) ) ;
#4670 = DIRECTION ( 'NONE',  ( -0.000000000000000000, -0.000000000000000000, 1.000000000000000000 ) ) ;
#4672 = EDGE_CURVE ( 'NONE', #4507, #18169, #7222, .T. ) ;
#4671 = CARTESIAN_POINT ( 'NONE',  ( 18.97034911358585418, 18.97034911358578668, 13.33755215474602984 ) ) ;
#4673 = CARTESIAN_POINT ( 'NONE',  ( 19.78573162020705922, 19.78573162020699172, 13.61880215351699874 ) ) ;
#4674 = CARTESIAN_POINT ( 'NONE',  ( -5.734022625014068453, 38.61087488181074434, 10.34268409280109502 ) ) ;
#4675 = DIRECTION ( 'NONE',  ( 0.000000000000000000, 0.000000000000000000, 1.000000000000000000 ) ) ;
#4676 = CARTESIAN_POINT ( 'NONE',  ( 3.756430356250004099, 28.89062499938548356, 6.831223922626973533 ) ) ;
#4678 = VERTEX_POINT ( 'NONE', #2462 ) ;
#4677 = CYLINDRICAL_SURFACE ( 'NONE', #12471, 0.5000000000000004441 ) ;
#4679 = CIRCLE ( 'NONE', #21812, 31.10000000000000142 ) ;
#4680 =( BOUNDED_CURVE ( )  B_SPLINE_CURVE ( 2, ( #13278, #13159, #23476, #21250, #19154, #3333, #9090, #10923, #3087 ),
 .UNSPECIFIED., .F., .F. ) 
 B_SPLINE_CURVE_WITH_KNOTS ( ( 3, 2, 2, 2, 3 ),
 ( 0.1749999999999999889, 0.1833333333333333204, 0.2000000000000000111, 0.2166666666666666741, 0.2250000000000000056 ),
 .UNSPECIFIED. ) 
 CURVE ( )  GEOMETRIC_REPRESENTATION_ITEM ( )  RATIONAL_B_SPLINE_CURVE ( ( 0.9330127018922194093, 0.9330127018922194093, 1.000000000000000000, 0.8660254037844387076, 1.000000000000000000, 0.8660254037844387076, 1.000000000000000000, 0.9330127018922194093, 0.9330127018922194093 ) ) 
 REPRESENTATION_ITEM ( '' )  );
#4681 = CARTESIAN_POINT ( 'NONE',  ( 18.01575495898401513, 18.01575495898394763, 13.33755215474603162 ) ) ;
#4682 = LINE ( 'NONE', #634, #16730 ) ;
#4683 = ORIENTED_EDGE ( 'NONE', *, *, #25754, .F. ) ;
#4684 = DIRECTION ( 'NONE',  ( 0.000000000000000000, 0.000000000000000000, 1.000000000000000000 ) ) ;
#4685 = CARTESIAN_POINT ( 'NONE',  ( -3.999999999999996447, 28.76874999877096784, 8.999999999999992895 ) ) ;
#4686 = CARTESIAN_POINT ( 'NONE',  ( -1.878215178125004048, -27.46562499938548640, 5.746835883940462963 ) ) ;
#4688 = VERTEX_POINT ( 'NONE', #20772 ) ;
#4687 = CYLINDRICAL_SURFACE ( 'NONE', #11242, 0.5000000000000004441 ) ;
#4689 = AXIS2_PLACEMENT_3D ( 'NONE', #5247, #1331, #17673 ) ;
#4690 = CARTESIAN_POINT ( 'NONE',  ( 18.83113746560522728, 18.83113746560514912, 12.99999999999999112 ) ) ;
#4691 = AXIS2_PLACEMENT_3D ( 'NONE', #18690, #4318, #14269 ) ;
#4692 = EDGE_CURVE ( 'NONE', #23209, #16529, #5138, .T. ) ;
#4693 = ORIENTED_EDGE ( 'NONE', *, *, #13161, .T. ) ;
#4694 = CARTESIAN_POINT ( 'NONE',  ( -3.756430356250003655, -26.94062499938548427, 8.999999999999992895 ) ) ;
#4695 = ORIENTED_EDGE ( 'NONE', *, *, #15699, .F. ) ;
#4696 = AXIS2_PLACEMENT_3D ( 'NONE', #1775, #25566, #17722 ) ;
#4697 = ORIENTED_EDGE ( 'NONE', *, *, #21958, .F. ) ;
#4698 = EDGE_CURVE ( 'NONE', #7162, #14796, #24441, .T. ) ;
#4699 = DIRECTION ( 'NONE',  ( -0.000000000000000000, -0.000000000000000000, 1.000000000000000000 ) ) ;
#4701 = DIRECTION ( 'NONE',  ( -0.7071067811865487940, -0.7071067811865463515, 0.000000000000000000 ) ) ;
#4700 = AXIS2_PLACEMENT_3D ( 'NONE', #18533, #226, #14353 ) ;
#4702 = B_SPLINE_CURVE_WITH_KNOTS ( 'NONE', 3,
 ( #9619, #1124, #19164, #23224, #3210, #21137, #3600, #11180, #17598, #15376, #1257, #25576, #9241, #13286, #13669, #21400, #21262, #17466 ),
 .UNSPECIFIED., .F., .F.,
 ( 4, 2, 2, 2, 2, 2, 2, 2, 4 ),
 ( 0.01878087663358380885, 0.01956282976579720376, 0.02034478289801060213, 0.02112673603022399704, 0.02190868916243739195, 0.02269064229465078686, 0.02347259542686418177, 0.02425454855907758014, 0.02503650169129097505 ),
 .UNSPECIFIED. ) ;
#4703 = CARTESIAN_POINT ( 'NONE',  ( 2.620986760973688460E-15, -13.61880215351699874, 3.431249998770965703 ) ) ;
#4704 = EDGE_CURVE ( 'NONE', #22201, #5837, #13488, .T. ) ;
#4705 = VECTOR ( 'NONE', #3620, 1000.000000000000000 ) ;
#4706 = CARTESIAN_POINT ( 'NONE',  ( 1.878215178125000939, -12.25316411605952283, 1.078124999385483784 ) ) ;
#4707 = DIRECTION ( 'NONE',  ( -0.000000000000000000, -1.000000000000000000, 0.000000000000000000 ) ) ;
#4708 = CARTESIAN_POINT ( 'NONE',  ( 2.672651547586948120E-15, 29.52812499938548285, 13.33755215474602984 ) ) ;
#4709 = AXIS2_PLACEMENT_3D ( 'NONE', #21206, #3285, #1198 ) ;
#4710 = ADVANCED_FACE ( 'NONE', ( #12925 ), #385, .T. ) ;
#4711 = CARTESIAN_POINT ( 'NONE',  ( 19.43607991388988765, 24.27856662945500688, -2.750000000000000000 ) ) ;
#4712 = CARTESIAN_POINT ( 'NONE',  ( -17.08421000182795879, -25.98730014090424234, -6.500000000000000000 ) ) ;
#4713 = UNCERTAINTY_MEASURE_WITH_UNIT (LENGTH_MEASURE( 1.000000000000000082E-05 ), #3407, 'distance_accuracy_value', 'NONE');
#4714 = CARTESIAN_POINT ( 'NONE',  ( -3.756430356249997438, 29.45312499938548356, 11.16877607737301048 ) ) ;
#4715 = CARTESIAN_POINT ( 'NONE',  ( 18.34500155353947903, 21.17342867828559605, 12.46410161513774639 ) ) ;
#4716 = DIRECTION ( 'NONE',  ( -1.000000000000000000, 0.000000000000000000, 0.000000000000000000 ) ) ;
#4717 = CARTESIAN_POINT ( 'NONE',  ( 2.000000000000003997, -5.535898384862238508, 0.9187499987709686344 ) ) ;
#4718 = CARTESIAN_POINT ( 'NONE',  ( -2.672651547586948120E-15, -26.04062499938548925, 13.33755215474602984 ) ) ;
#4719 = CARTESIAN_POINT ( 'NONE',  ( -1.878215178124998497, 29.60312499938548569, 12.25316411605951927 ) ) ;
#4720 = DIRECTION ( 'NONE',  ( 1.000000000000000000, 0.000000000000000000, 0.000000000000000000 ) ) ;
#4721 = CARTESIAN_POINT ( 'NONE',  ( -29.62293631110035363, 7.734255490827311341, -6.500000000000000000 ) ) ;
#4722 = CARTESIAN_POINT ( 'NONE',  ( 2.644755406393140440, -29.88376691385261097, 5.987824696368042154 ) ) ;
#4723 = ORIENTED_EDGE ( 'NONE', *, *, #7399, .F. ) ;
#4724 = FACE_OUTER_BOUND ( 'NONE', #5151, .T. ) ;
#4726 = ORIENTED_EDGE ( 'NONE', *, *, #4522, .T. ) ;
#4725 = DIRECTION ( 'NONE',  ( 1.000000000000000000, 0.000000000000000000, 0.000000000000000000 ) ) ;
#4727 = CIRCLE ( 'NONE', #12217, 31.10000000000000142 ) ;
#4728 = VERTEX_POINT ( 'NONE', #18428 ) ;
#4729 = ORIENTED_EDGE ( 'NONE', *, *, #10657, .F. ) ;
#4730 = VERTEX_POINT ( 'NONE', #524 ) ;
#4731 = VERTEX_POINT ( 'NONE', #20645 ) ;
#4732 = CARTESIAN_POINT ( 'NONE',  ( -5.577813053751546416E-15, -25.33750000000000213, 12.99999999999999289 ) ) ;
#4733 = VECTOR ( 'NONE', #21060, 1000.000000000000000 ) ;
#4734 = ORIENTED_EDGE ( 'NONE', *, *, #362, .F. ) ;
#4735 = EDGE_CURVE ( 'NONE', #19594, #15159, #18564, .T. ) ;
#4736 = DIRECTION ( 'NONE',  ( 1.000000000000000000, 0.000000000000000000, 0.000000000000000000 ) ) ;
#4737 = CARTESIAN_POINT ( 'NONE',  ( 3.756430356250002323, 28.36562499938548854, 11.16877607737301403 ) ) ;
#4738 =( BOUNDED_CURVE ( )  B_SPLINE_CURVE ( 2, ( #10994, #1059, #16762, #12430, #22774, #555, #16897, #4456, #24861 ),
 .UNSPECIFIED., .F., .F. ) 
 B_SPLINE_CURVE_WITH_KNOTS ( ( 3, 2, 2, 2, 3 ),
 ( 0.5750000000000000666, 0.5833333333333333703, 0.5999999999999999778, 0.6166666666666666963, 0.6250000000000000000 ),
 .UNSPECIFIED. ) 
 CURVE ( )  GEOMETRIC_REPRESENTATION_ITEM ( )  RATIONAL_B_SPLINE_CURVE ( ( 0.9330127018922194093, 0.9330127018922198534, 1.000000000000000000, 0.8660254037844387076, 1.000000000000000000, 0.8660254037844387076, 1.000000000000000000, 0.9330127018922194093, 0.9330127018922194093 ) ) 
 REPRESENTATION_ITEM ( '' )  );
#4739 = EDGE_CURVE ( 'NONE', #17107, #4508, #16825, .T. ) ;
#4740 = CARTESIAN_POINT ( 'NONE',  ( 3.756430356250004099, -6.831223922626973533, 1.640624999385484895 ) ) ;
#4741 = DIRECTION ( 'NONE',  ( -0.000000000000000000, -0.000000000000000000, 1.000000000000000000 ) ) ;
#4742 = CARTESIAN_POINT ( 'NONE',  ( 18.78246010926947918, 21.43865748722877740, 5.746835883940462963 ) ) ;
#4743 = ADVANCED_FACE ( 'NONE', ( #25338 ), #3364, .T. ) ;
#4744 = DIRECTION ( 'NONE',  ( -0.000000000000000000, 0.000000000000000000, 1.000000000000000000 ) ) ;
#4745 = PRESENTATION_LAYER_ASSIGNMENT (  '', '', ( #8495 ) ) ;
#4746 = EDGE_CURVE ( 'NONE', #16889, #17313, #10902, .T. ) ;
#4747 = LINE ( 'NONE', #18862, #19222 ) ;
#4748 = CARTESIAN_POINT ( 'NONE',  ( -3.756430356249996994, -8.999999999999992895, 4.415624999385483918 ) ) ;
#4749 = DIRECTION ( 'NONE',  ( 1.000000000000000000, 0.000000000000000000, 0.000000000000000000 ) ) ;
#4750 = CARTESIAN_POINT ( 'NONE',  ( -1.999999999999998224, -12.46410161513774639, 3.900000000000000799 ) ) ;
#4751 = CARTESIAN_POINT ( 'NONE',  ( 1.500000000000001776, -10.49999999999999289, -6.938893903907228378E-15 ) ) ;
#4752 = DIRECTION ( 'NONE',  ( 0.000000000000000000, 0.000000000000000000, 1.000000000000000000 ) ) ;
#4753 = CARTESIAN_POINT ( 'NONE',  ( 3.756430356250003655, -8.999999999999992895, 2.953124999385485339 ) ) ;
#4754 = CYLINDRICAL_SURFACE ( 'NONE', #13284, 0.5000000000000004441 ) ;
#4755 = EDGE_CURVE ( 'NONE', #9389, #4038, #4727, .T. ) ;
#4756 = LINE ( 'NONE', #5957, #2615 ) ;
#4757 = ORIENTED_EDGE ( 'NONE', *, *, #20870, .F. ) ;
#4758 = ORIENTED_EDGE ( 'NONE', *, *, #25197, .T. ) ;
#4759 = CARTESIAN_POINT ( 'NONE',  ( -1.878215178124996498, 29.00312499938548783, 5.746835883940462963 ) ) ;
#4760 = ORIENTED_EDGE ( 'NONE', *, *, #19981, .F. ) ;
#4761 = CYLINDRICAL_SURFACE ( 'NONE', #9192, 0.5000000000000004441 ) ;
#4762 = ORIENTED_EDGE ( 'NONE', *, *, #13106, .T. ) ;
#4763 = CARTESIAN_POINT ( 'NONE',  ( 3.756430356249995661, -25.89062499938548356, 6.831223922626973533 ) ) ;
#4764 = ORIENTED_EDGE ( 'NONE', *, *, #12435, .F. ) ;
#4765 = FACE_OUTER_BOUND ( 'NONE', #4383, .T. ) ;
#4766 = ORIENTED_EDGE ( 'NONE', *, *, #16566, .T. ) ;
#4767 = CARTESIAN_POINT ( 'NONE',  ( 3.526711513754818395, 29.50000000000000000, 4.645898033750289535 ) ) ;
#4768 = CARTESIAN_POINT ( 'NONE',  ( 2.000000000000000888, 25.82499999999999929, 12.46410161513774817 ) ) ;
#4769 = EDGE_CURVE ( 'NONE', #10104, #4609, #21158, .T. ) ;
#4770 = DIRECTION ( 'NONE',  ( 0.000000000000000000, 0.000000000000000000, 1.000000000000000000 ) ) ;
#4771 = DIRECTION ( 'NONE',  ( 0.000000000000000000, 0.000000000000000000, 1.000000000000000000 ) ) ;
#4772 = CARTESIAN_POINT ( 'NONE',  ( 18.25440349763447756, 18.25440349763440295, 4.662447845253954171 ) ) ;
#4773 = CARTESIAN_POINT ( 'NONE',  ( 1.878215178125000939, 28.21562499938548640, 12.25316411605952283 ) ) ;
#4774 = EDGE_CURVE ( 'NONE', #1139, #25560, #14325, .T. ) ;
#4775 = CARTESIAN_POINT ( 'NONE',  ( 8.831537335106614961E-15, 26.23749999999999716, 12.99999999999999112 ) ) ;
#4776 = CARTESIAN_POINT ( 'NONE',  ( 2.000000000000000888, 26.66874999877096641, 12.46410161513774817 ) ) ;
#4777 = DIRECTION ( 'NONE',  ( 0.9822872507286884991, -0.1873813145857256834, 0.000000000000000000 ) ) ;
#4778 = CARTESIAN_POINT ( 'NONE',  ( 4.000000000000002665, 26.33124999877097494, 6.690598923241489970 ) ) ;
#4779 = DIRECTION ( 'NONE',  ( 1.000000000000000000, 0.000000000000000000, 0.000000000000000000 ) ) ;
#4780 = CARTESIAN_POINT ( 'NONE',  ( 1.878215178124995832, -27.99062499938548143, 5.746835883940462963 ) ) ;
#4781 = CARTESIAN_POINT ( 'NONE',  ( 3.999999999999976019, -11.30940107675851536, 0.4124999999999983125 ) ) ;
#4782 = CARTESIAN_POINT ( 'NONE',  ( 1.878215178125000939, 26.52812499938548285, 12.25316411605952283 ) ) ;
#4783 = CARTESIAN_POINT ( 'NONE',  ( 2.665892461326258456, 29.88220662469441891, 11.99618178085344056 ) ) ;
#4785 = ORIENTED_EDGE ( 'NONE', *, *, #4423, .F. ) ;
#4784 = CARTESIAN_POINT ( 'NONE',  ( -1.878215178124996498, 29.45312499938548711, 5.746835883940462963 ) ) ;
#4786 = ORIENTED_EDGE ( 'NONE', *, *, #18920, .T. ) ;
#4787 = LINE ( 'NONE', #12880, #22930 ) ;
#4788 = PRODUCT_DEFINITION_FORMATION_WITH_SPECIFIED_SOURCE ( 'ANY', '', #7169, .NOT_KNOWN. ) ;
#4789 = CARTESIAN_POINT ( 'NONE',  ( 2.620986760973688460E-15, -13.61880215351699874, 4.331249998770966059 ) ) ;
#4790 = ORIENTED_EDGE ( 'NONE', *, *, #21668, .F. ) ;
#4791 = CARTESIAN_POINT ( 'NONE',  ( -3.756430356250003655, -27.05312499938548498, 8.999999999999992895 ) ) ;
#4792 = CARTESIAN_POINT ( 'NONE',  ( 3.756430356250002323, 29.60312499938548925, 11.16877607737301226 ) ) ;
#4793 = CARTESIAN_POINT ( 'NONE',  ( 1.878215178125003382, 26.11562499938548854, 5.746835883940462963 ) ) ;
#4794 = CARTESIAN_POINT ( 'NONE',  ( 1.859271017917182139E-15, 26.18124999877096570, 12.99999999999999289 ) ) ;
#4795 = CARTESIAN_POINT ( 'NONE',  ( 3.756430356250003211, 26.94062499938548783, 8.999999999999992895 ) ) ;
#4796 = CARTESIAN_POINT ( 'NONE',  ( -1.999999999999994893, 28.75000000000000355, 5.535898384862237620 ) ) ;
#4797 = EDGE_CURVE ( 'NONE', #22637, #13892, #21838, .T. ) ;
#4798 = CARTESIAN_POINT ( 'NONE',  ( 23.35662086519912606, 17.69976661570667176, 6.690598923241489970 ) ) ;
#4799 = CYLINDRICAL_SURFACE ( 'NONE', #820, 4.000000000000000000 ) ;
#4800 = CARTESIAN_POINT ( 'NONE',  ( -29.99470236596038220, -8.217531866530892515, 1.000000000000000000 ) ) ;
#4801 = FACE_OUTER_BOUND ( 'NONE', #9566, .T. ) ;
#4802 = MANIFOLD_SOLID_BREP ( 'Cavity1', #11284 ) ;
#4803 = CARTESIAN_POINT ( 'NONE',  ( 18.83113746560522728, 18.83113746560514912, 12.99999999999999112 ) ) ;
#4804 = CARTESIAN_POINT ( 'NONE',  ( 22.02429405596265610, 16.71189930004383584, 8.999999999999992895 ) ) ;
#4805 = CARTESIAN_POINT ( 'NONE',  ( 15.33304107673014727, 20.64543583264882542, 6.831223922626973533 ) ) ;
#4806 = DIRECTION ( 'NONE',  ( -0.000000000000000000, 0.000000000000000000, 1.000000000000000000 ) ) ;
#4807 = EDGE_CURVE ( 'NONE', #22201, #23568, #15665, .T. ) ;
#4808 = CARTESIAN_POINT ( 'NONE',  ( -3.756430356249997882, 26.75312499938548427, 11.16877607737301226 ) ) ;
#4809 = DIRECTION ( 'NONE',  ( -0.000000000000000000, -0.000000000000000000, 1.000000000000000000 ) ) ;
#4810 = CARTESIAN_POINT ( 'NONE',  ( 21.09621640565530853, 15.78382164973649537, 6.831223922626973533 ) ) ;
#4811 = CARTESIAN_POINT ( 'NONE',  ( 24.27856662945494293, -19.43607991388997291, 1.000000000000000000 ) ) ;
#4812 = VERTEX_POINT ( 'NONE', #23506 ) ;
#4813 = DIRECTION ( 'NONE',  ( 0.000000000000000000, 0.000000000000000000, 1.000000000000000000 ) ) ;
#4814 = CARTESIAN_POINT ( 'NONE',  ( -1.999999999999998224, 27.94374999877096855, 12.46410161513774639 ) ) ;
#4815 = CARTESIAN_POINT ( 'NONE',  ( 1.878215178124995832, -25.74062499938548498, 5.746835883940462963 ) ) ;
#4816 = VERTEX_POINT ( 'NONE', #19946 ) ;
#4817 = CARTESIAN_POINT ( 'NONE',  ( 15.89664432368105551, 21.55349857317336415, 6.690598923241487306 ) ) ;
#4818 = EDGE_LOOP ( 'NONE', ( #15663, #3549, #7018, #4869 ) ) ;
#4819 = CARTESIAN_POINT ( 'NONE',  ( -3.756430356250003655, -25.59062499938548285, 8.999999999999992895 ) ) ;
#4820 = EDGE_LOOP ( 'NONE', ( #25713, #19268, #14049, #4450 ) ) ;
#4821 = ORIENTED_EDGE ( 'NONE', *, *, #6192, .T. ) ;
#4822 = CARTESIAN_POINT ( 'NONE',  ( 4.006172263299091013E-15, 27.16562499938548569, 4.662447845253954171 ) ) ;
#4823 = DIRECTION ( 'NONE',  ( -0.000000000000000000, -0.000000000000000000, 1.000000000000000000 ) ) ;
#4824 = EDGE_CURVE ( 'NONE', #15750, #15689, #19308, .T. ) ;
#4825 = CARTESIAN_POINT ( 'NONE',  ( 1.878215178125004048, -5.746835883940462963, 3.028124999385484184 ) ) ;
#4826 = LINE ( 'NONE', #909, #1352 ) ;
#4827 = CARTESIAN_POINT ( 'NONE',  ( -1.878215178124995832, 27.54062499938548214, 5.746835883940462963 ) ) ;
#4828 = EDGE_CURVE ( 'NONE', #17442, #24369, #22045, .T. ) ;
#4829 = DIRECTION ( 'NONE',  ( 0.000000000000000000, 0.000000000000000000, 1.000000000000000000 ) ) ;
#4830 = CARTESIAN_POINT ( 'NONE',  ( 3.999999999999996447, -28.82499999999999929, 8.999999999999992895 ) ) ;
#4831 = AXIS2_PLACEMENT_3D ( 'NONE', #11942, #24239, #14442 ) ;
#4832 = CARTESIAN_POINT ( 'NONE',  ( 1.878215178125000939, 29.56562499938548427, 12.25316411605952283 ) ) ;
#4833 = CARTESIAN_POINT ( 'NONE',  ( 19.78573162020706988, 19.78573162020698462, 12.99999999999999289 ) ) ;
#4834 = DIRECTION ( 'NONE',  ( 0.000000000000000000, 0.000000000000000000, 1.000000000000000000 ) ) ;
#4835 = FACE_OUTER_BOUND ( 'NONE', #1448, .T. ) ;
#4836 = ADVANCED_FACE ( 'NONE', ( #17749 ), #11590, .T. ) ;
#4837 = CARTESIAN_POINT ( 'NONE',  ( -3.756430356250002323, -27.01562499938548356, 11.16877607737301226 ) ) ;
#4838 = CARTESIAN_POINT ( 'NONE',  ( 3.756430356250004099, 25.29062499938548569, 6.831223922626973533 ) ) ;
#4839 = CARTESIAN_POINT ( 'NONE',  ( 8.831537335106614961E-15, 27.53124999877097068, 12.99999999999999112 ) ) ;
#4840 = DIRECTION ( 'NONE',  ( -0.000000000000000000, -0.000000000000000000, 1.000000000000000000 ) ) ;
#4841 = CARTESIAN_POINT ( 'NONE',  ( -31.00322564728516639, -2.451530025008796798, 1.000000000000000000 ) ) ;
#4842 = ORIENTED_EDGE ( 'NONE', *, *, #22461, .T. ) ;
#4843 = EDGE_CURVE ( 'NONE', #19911, #19004, #5155, .T. ) ;
#4844 = CARTESIAN_POINT ( 'NONE',  ( -3.959305671612554781E-15, -30.00000000000000355, 12.99999999999999289 ) ) ;
#4846 = ORIENTED_EDGE ( 'NONE', *, *, #3638, .T. ) ;
#4845 = CARTESIAN_POINT ( 'NONE',  ( 14.98253926456319007, -27.25313774936425304, -6.500000000000000000 ) ) ;
#4847 = ORIENTED_EDGE ( 'NONE', *, *, #3569, .F. ) ;
#4848 = MANIFOLD_SOLID_BREP ( 'CirPattern3', #1707 ) ;
#4849 = ORIENTED_EDGE ( 'NONE', *, *, #17515, .F. ) ;
#4850 = VERTEX_POINT ( 'NONE', #11858 ) ;
#4851 = ORIENTED_EDGE ( 'NONE', *, *, #239, .F. ) ;
#4852 = DIRECTION ( 'NONE',  ( 0.000000000000000000, 0.000000000000000000, 1.000000000000000000 ) ) ;
#4853 = VERTEX_POINT ( 'NONE', #9889 ) ;
#4854 = CYLINDRICAL_SURFACE ( 'NONE', #24875, 1.500000000000000222 ) ;
#4855 = CARTESIAN_POINT ( 'NONE',  ( 3.756430356250003655, 29.30312499938548498, 8.999999999999992895 ) ) ;
#4856 = CARTESIAN_POINT ( 'NONE',  ( 1.878215178125004048, -5.746835883940462963, 1.115624999385483207 ) ) ;
#4857 = FACE_OUTER_BOUND ( 'NONE', #4617, .T. ) ;
#4858 = DIRECTION ( 'NONE',  ( 0.000000000000000000, 0.000000000000000000, 1.000000000000000000 ) ) ;
#4859 = CARTESIAN_POINT ( 'NONE',  ( 3.756430356250004099, 25.74062499938548143, 6.831223922626973533 ) ) ;
#4860 = CARTESIAN_POINT ( 'NONE',  ( -6.741346781237202102, -25.16843286583315731, 20.00001200000000168 ) ) ;
#4861 = CARTESIAN_POINT ( 'NONE',  ( -3.999999999999996003, -6.690598923241487306, 0.1875000000000008882 ) ) ;
#4862 = DIRECTION ( 'NONE',  ( -0.000000000000000000, -0.000000000000000000, -1.000000000000000000 ) ) ;
#4863 = DIRECTION ( 'NONE',  ( -0.8090169943749417891, 0.5877852522924807976, 0.000000000000000000 ) ) ;
#4864 = CARTESIAN_POINT ( 'NONE',  ( 9.610428525060889626, 29.57785765677927614, 1.000000000000000000 ) ) ;
#4865 = CARTESIAN_POINT ( 'NONE',  ( 3.369928719974892281E-15, 25.11250000000000426, 4.999999999999992006 ) ) ;
#4866 = CARTESIAN_POINT ( 'NONE',  ( -3.756430356249996994, -8.999999999999992895, 2.278124999385483740 ) ) ;
#4867 = CARTESIAN_POINT ( 'NONE',  ( -1.071796769724487453, 25.13259618943234486, 4.999999999999992006 ) ) ;
#4868 = CARTESIAN_POINT ( 'NONE',  ( 3.526711513754818395, 29.50000000000000000, 4.145898033750289535 ) ) ;
#4869 = ORIENTED_EDGE ( 'NONE', *, *, #4942, .F. ) ;
#4870 = EDGE_CURVE ( 'NONE', #383, #5108, #25721, .T. ) ;
#4871 = ORIENTED_EDGE ( 'NONE', *, *, #14360, .F. ) ;
#4872 = CARTESIAN_POINT ( 'NONE',  ( -1.878215178124996498, 27.65312499938548996, 5.746835883940462963 ) ) ;
#4873 = EDGE_CURVE ( 'NONE', #23529, #8768, #16019, .T. ) ;
#4874 = ORIENTED_EDGE ( 'NONE', *, *, #17793, .T. ) ;
#4875 = LINE ( 'NONE', #7231, #16229 ) ;
#4876 = ORIENTED_EDGE ( 'NONE', *, *, #17614, .F. ) ;
#4877 = CARTESIAN_POINT ( 'NONE',  ( 1.878215178124998497, -25.55312499938548854, 12.25316411605951927 ) ) ;
#4878 = ORIENTED_EDGE ( 'NONE', *, *, #10953, .F. ) ;
#4879 = CARTESIAN_POINT ( 'NONE',  ( -16.23990935651680090, 26.52310962334767908, -6.500000000000000000 ) ) ;
#4880 =( BOUNDED_CURVE ( )  B_SPLINE_CURVE ( 2, ( #263, #17785, #22082, #8229, #6264, #24176, #20123, #16204, #25752 ),
 .UNSPECIFIED., .F., .F. ) 
 B_SPLINE_CURVE_WITH_KNOTS ( ( 3, 2, 2, 2, 3 ),
 ( 0.2250000000000000056, 0.2333333333333333370, 0.2500000000000000000, 0.2666666666666666630, 0.2750000000000000222 ),
 .UNSPECIFIED. ) 
 CURVE ( )  GEOMETRIC_REPRESENTATION_ITEM ( )  RATIONAL_B_SPLINE_CURVE ( ( 0.9330127018922194093, 0.9330127018922194093, 1.000000000000000000, 0.8660254037844387076, 1.000000000000000000, 0.8660254037844387076, 1.000000000000000000, 0.9330127018922191873, 0.9330127018922194093 ) ) 
 REPRESENTATION_ITEM ( '' )  );
#4881 = ORIENTED_EDGE ( 'NONE', *, *, #16934, .F. ) ;
#4882 = DIRECTION ( 'NONE',  ( 0.5358267949789962126, -0.8443279255020154084, 0.000000000000000000 ) ) ;
#4883 = CARTESIAN_POINT ( 'NONE',  ( 2.000000000000003997, 25.07499999999999929, 5.535898384862238508 ) ) ;
#4884 = DIRECTION ( 'NONE',  ( 0.8090169943749532244, 0.5877852522924652545, 0.000000000000000000 ) ) ;
#4885 = DIRECTION ( 'NONE',  ( 0.000000000000000000, 0.000000000000000000, 1.000000000000000000 ) ) ;
#4886 = CARTESIAN_POINT ( 'NONE',  ( -1.999999999999995781, 28.24374999877096570, 5.535898384862237620 ) ) ;
#4887 = CARTESIAN_POINT ( 'NONE',  ( 18.33167953626305646, 20.98787691422236179, 12.25316411605951927 ) ) ;
#4888 = LINE ( 'NONE', #11419, #5849 ) ;
#4889 = CARTESIAN_POINT ( 'NONE',  ( -3.756430356249996994, 28.96562499938548285, 8.999999999999992895 ) ) ;
#4890 = LINE ( 'NONE', #22297, #2172 ) ;
#4891 = DIRECTION ( 'NONE',  ( 0.000000000000000000, 0.000000000000000000, 1.000000000000000000 ) ) ;
#4892 = EDGE_CURVE ( 'NONE', #9493, #2390, #19718, .T. ) ;
#4893 = VERTEX_POINT ( 'NONE', #21388 ) ;
#4894 = CARTESIAN_POINT ( 'NONE',  ( 26.00000000000000355, 1.592040838891558898E-15, 20.00000599999999906 ) ) ;
#4895 = CARTESIAN_POINT ( 'NONE',  ( 6.009258394948636914E-15, 26.40624999877097423, 4.381197846482986158 ) ) ;
#4897 = EDGE_CURVE ( 'NONE', #5989, #9673, #8077, .T. ) ;
#4896 = CARTESIAN_POINT ( 'NONE',  ( -1.878215178125004048, -26.56562499938548427, 5.746835883940462963 ) ) ;
#4898 = DIRECTION ( 'NONE',  ( -0.000000000000000000, -0.000000000000000000, 1.000000000000000000 ) ) ;
#4899 = CARTESIAN_POINT ( 'NONE',  ( 1.878215178125000939, 25.62812499938548783, 12.25316411605952283 ) ) ;
#4900 = LINE ( 'NONE', #11041, #15475 ) ;
#4902 = ORIENTED_EDGE ( 'NONE', *, *, #11344, .T. ) ;
#4901 = CARTESIAN_POINT ( 'NONE',  ( 3.756430356250004099, 29.34062499938548640, 6.831223922626973533 ) ) ;
#4903 = ORIENTED_EDGE ( 'NONE', *, *, #9378, .F. ) ;
#4904 = CARTESIAN_POINT ( 'NONE',  ( 1.878215178125000939, 29.67812499938548498, 12.25316411605952283 ) ) ;
#4905 = DIRECTION ( 'NONE',  ( -0.000000000000000000, -1.000000000000000000, -0.000000000000000000 ) ) ;
#4906 = ORIENTED_EDGE ( 'NONE', *, *, #16902, .F. ) ;
#4907 = CARTESIAN_POINT ( 'NONE',  ( -3.756430356250002323, -29.26562499938548356, 11.16877607737301403 ) ) ;
#4908 = LINE ( 'NONE', #8978, #21807 ) ;
#4909 = CARTESIAN_POINT ( 'NONE',  ( -2.003086131649545506E-15, 26.82812499938549067, 13.33755215474603162 ) ) ;
#4910 = DIRECTION ( 'NONE',  ( 0.000000000000000000, 0.000000000000000000, 1.000000000000000000 ) ) ;
#4911 = CARTESIAN_POINT ( 'NONE',  ( 4.000000000000002665, 25.86250000000000071, 11.30940107675849760 ) ) ;
#4912 = CARTESIAN_POINT ( 'NONE',  ( 0.7500000000000001110, 0.000000000000000000, 17.69999999999999929 ) ) ;
#4913 = CARTESIAN_POINT ( 'NONE',  ( 0.7500000000000001110, 1.299038105676658450, 17.69999999999999929 ) ) ;
#4914 = CARTESIAN_POINT ( 'NONE',  ( 0.000000000000000000, 0.000000000000000000, 20.00000000000000000 ) ) ;
#4915 = CARTESIAN_POINT ( 'NONE',  ( 16.59933168835424411, 22.25618593784655630, 8.999999999999992895 ) ) ;
#4916 = CARTESIAN_POINT ( 'NONE',  ( -23.64116323484252291, -20.20656826142258211, 1.000000000000000000 ) ) ;
#4917 = FACE_OUTER_BOUND ( 'NONE', #9792, .T. ) ;
#4918 = CARTESIAN_POINT ( 'NONE',  ( 24.27856662945494293, -19.43607991388997291, -6.500000000000000000 ) ) ;
#4919 = CARTESIAN_POINT ( 'NONE',  ( 23.32360276639294128, 18.01120801047411746, 6.831223922626973533 ) ) ;
#4920 = CARTESIAN_POINT ( 'NONE',  ( 19.04989862646933929, 19.04989862646927534, 13.33755215474602984 ) ) ;
#4921 = CARTESIAN_POINT ( 'NONE',  ( -3.469446951953614189E-15, -30.00000000000000355, 8.999999999999992895 ) ) ;
#4922 = EDGE_CURVE ( 'NONE', #22272, #17660, #22392, .T. ) ;
#4923 = DIRECTION ( 'NONE',  ( 1.000000000000000000, 0.000000000000000000, 0.000000000000000000 ) ) ;
#4924 = CARTESIAN_POINT ( 'NONE',  ( -3.756430356249996994, 28.06562499938548427, 8.999999999999992895 ) ) ;
#4925 = DIRECTION ( 'NONE',  ( 0.000000000000000000, 0.000000000000000000, 1.000000000000000000 ) ) ;
#4926 = CARTESIAN_POINT ( 'NONE',  ( 18.57032807491351178, 21.22652545287281356, 12.25316411605951927 ) ) ;
#4927 = DIRECTION ( 'NONE',  ( 0.000000000000000000, -1.000000000000000000, 0.000000000000000000 ) ) ;
#4928 = CIRCLE ( 'NONE', #10776, 0.4999999999999983902 ) ;
#4929 = VERTEX_POINT ( 'NONE', #6997 ) ;
#4930 = FACE_OUTER_BOUND ( 'NONE', #6315, .T. ) ;
#4931 = CARTESIAN_POINT ( 'NONE',  ( -1.999999999999998224, 27.04374999877096641, 12.46410161513774639 ) ) ;
#4932 = CARTESIAN_POINT ( 'NONE',  ( 3.756430356249997882, -28.10312499938548569, 11.16877607737301226 ) ) ;
#4934 = ORIENTED_EDGE ( 'NONE', *, *, #2469, .F. ) ;
#4933 = DIRECTION ( 'NONE',  ( -0.5877852522924652545, 0.8090169943749532244, 0.000000000000000000 ) ) ;
#4935 = LINE ( 'NONE', #8729, #18745 ) ;
#4936 = ADVANCED_FACE ( 'NONE', ( #14981 ), #5044, .T. ) ;
#4937 = VERTEX_POINT ( 'NONE', #9603 ) ;
#4938 = CARTESIAN_POINT ( 'NONE',  ( -3.756430356250004099, -28.77812499938548285, 6.831223922626973533 ) ) ;
#4939 = EDGE_LOOP ( 'NONE', ( #11298, #8517, #13447, #17687 ) ) ;
#4940 = VERTEX_POINT ( 'NONE', #23716 ) ;
#4941 = CARTESIAN_POINT ( 'NONE',  ( 3.756430356250002323, 27.91562499938548925, 11.16877607737301226 ) ) ;
#4942 = EDGE_CURVE ( 'NONE', #10748, #19630, #7511, .T. ) ;
#4943 = VECTOR ( 'NONE', #20295, 1000.000000000000000 ) ;
#4944 = CARTESIAN_POINT ( 'NONE',  ( 0.000000000000000000, 0.000000000000000000, -6.500000000000000000 ) ) ;
#4945 =( BOUNDED_CURVE ( )  B_SPLINE_CURVE ( 2, ( #19190, #17119, #13458, #15670, #1288, #21292, #9650, #19572, #23638 ),
 .UNSPECIFIED., .F., .T. ) 
 B_SPLINE_CURVE_WITH_KNOTS ( ( 3, 2, 2, 2, 3 ),
 ( 0.4750000000000000333, 0.4833333333333333370, 0.5000000000000000000, 0.5166666666666667185, 0.5250000000000000222 ),
 .UNSPECIFIED. ) 
 CURVE ( )  GEOMETRIC_REPRESENTATION_ITEM ( )  RATIONAL_B_SPLINE_CURVE ( ( 0.9330127018922194093, 0.9330127018922196314, 1.000000000000000000, 0.8660254037844387076, 1.000000000000000000, 0.8660254037844387076, 1.000000000000000000, 0.9330127018922194093, 0.9330127018922194093 ) ) 
 REPRESENTATION_ITEM ( '' )  );
#4946 = CIRCLE ( 'NONE', #8291, 31.10000000000000142 ) ;
#4947 = CIRCLE ( 'NONE', #25000, 0.4999999999999991673 ) ;
#4948 = CARTESIAN_POINT ( 'NONE',  ( 3.756430356250004099, -6.831223922626973533, 1.190624999385485383 ) ) ;
#4949 =( NAMED_UNIT ( * ) PLANE_ANGLE_UNIT ( ) SI_UNIT ( $, .RADIAN. ) );
#4950 = CARTESIAN_POINT ( 'NONE',  ( 19.43607991388981304, -24.27856662945506727, 1.000000000000000000 ) ) ;
#4951 = CARTESIAN_POINT ( 'NONE',  ( 3.735045420075836212E-15, 27.95312499938548001, 4.662447845253954171 ) ) ;
#4952 = LINE ( 'NONE', #12934, #21750 ) ;
#4953 = CARTESIAN_POINT ( 'NONE',  ( -26.52310962334728828, 16.23990935651745460, 1.000000000000000000 ) ) ;
#4954 = UNCERTAINTY_MEASURE_WITH_UNIT (LENGTH_MEASURE( 1.000000000000000082E-05 ), #6137, 'distance_accuracy_value', 'NONE');
#4955 = UNCERTAINTY_MEASURE_WITH_UNIT (LENGTH_MEASURE( 1.000000000000000082E-05 ), #21934, 'distance_accuracy_value', 'NONE');
#4956 = CARTESIAN_POINT ( 'NONE',  ( 3.735045420075836212E-15, 28.85312499938548569, 4.662447845253954171 ) ) ;
#4957 = SURFACE_STYLE_FILL_AREA ( #22875 ) ;
#4958 = CARTESIAN_POINT ( 'NONE',  ( 0.000000000000000000, 0.000000000000000000, 19.59999999999999787 ) ) ;
#4959 = DIRECTION ( 'NONE',  ( -0.000000000000000000, -1.000000000000000000, -0.000000000000000000 ) ) ;
#4960 = CARTESIAN_POINT ( 'NONE',  ( 27.92360179968377309, 13.69242354489143842, -2.750000000000000000 ) ) ;
#4961 = CARTESIAN_POINT ( 'NONE',  ( 1.878215178124998497, -27.80312499938548498, 12.25316411605951927 ) ) ;
#4962 = CARTESIAN_POINT ( 'NONE',  ( 3.756430356250002323, 25.66562499938548569, 11.16877607737301226 ) ) ;
#4963 = LINE ( 'NONE', #5225, #24573 ) ;
#4964 = VECTOR ( 'NONE', #11221, 1000.000000000000000 ) ;
#4965 = DIRECTION ( 'NONE',  ( 0.000000000000000000, 0.000000000000000000, 1.000000000000000000 ) ) ;
#4966 = CARTESIAN_POINT ( 'NONE',  ( 21.69050051289738690, 18.86207338815112067, 5.535898384862238508 ) ) ;
#4968 = VERTEX_POINT ( 'NONE', #11829 ) ;
#4967 = AXIS2_PLACEMENT_3D ( 'NONE', #23011, #14780, #6798 ) ;
#4969 = DIRECTION ( 'NONE',  ( -0.000000000000000000, -0.000000000000000000, 1.000000000000000000 ) ) ;
#4971 = ORIENTED_EDGE ( 'NONE', *, *, #25125, .F. ) ;
#4970 = CYLINDRICAL_SURFACE ( 'NONE', #5408, 0.5000000000000004441 ) ;
#4972 = AXIS2_PLACEMENT_3D ( 'NONE', #482, #24404, #14855 ) ;
#4974 = ORIENTED_EDGE ( 'NONE', *, *, #16031, .F. ) ;
#4973 = ADVANCED_FACE ( 'NONE', ( #1897 ), #11560, .T. ) ;
#4976 = ORIENTED_EDGE ( 'NONE', *, *, #11344, .F. ) ;
#4975 = VECTOR ( 'NONE', #6768, 1000.000000000000000 ) ;
#4977 = EDGE_LOOP ( 'NONE', ( #8413, #2785, #3317, #23775, #21418, #7446, #23268, #15188, #18106, #13777, #12631, #5526, #9917, #9537, #5487, #11999, #1893, #15334, #14245, #10688, #2276, #25632, #5722 ) ) ;
#4978 = ORIENTED_EDGE ( 'NONE', *, *, #25575, .T. ) ;
#4979 = LINE ( 'NONE', #16623, #23902 ) ;
#4980 = ADVANCED_FACE ( 'NONE', ( #3980 ), #15753, .F. ) ;
#4981 = ORIENTED_EDGE ( 'NONE', *, *, #3174, .F. ) ;
#4982 = EDGE_CURVE ( 'NONE', #933, #9293, #9862, .T. ) ;
#4983 = CARTESIAN_POINT ( 'NONE',  ( 0.000000000000000000, 0.000000000000000000, -6.500000000000000000 ) ) ;
#4984 = CARTESIAN_POINT ( 'NONE',  ( 2.672651547586948120E-15, 29.64062499938548356, 13.33755215474603162 ) ) ;
#4985 = CARTESIAN_POINT ( 'NONE',  ( -3.756430356249996994, -8.999999999999992895, 4.528124999385485516 ) ) ;
#4986 = PRESENTATION_STYLE_ASSIGNMENT (( #14535 ) ) ;
#4987 = CARTESIAN_POINT ( 'NONE',  ( 23.00540471485899374, 17.69300995894016992, 6.831223922626973533 ) ) ;
#4988 = EDGE_CURVE ( 'NONE', #19150, #12673, #25199, .T. ) ;
#4989 = CARTESIAN_POINT ( 'NONE',  ( 2.672651547586948120E-15, 26.04062499938548925, 13.33755215474602984 ) ) ;
#4990 = DIRECTION ( 'NONE',  ( 0.000000000000000000, 0.000000000000000000, 1.000000000000000000 ) ) ;
#4991 = CIRCLE ( 'NONE', #2079, 0.5000000000000001110 ) ;
#4992 = CARTESIAN_POINT ( 'NONE',  ( -1.878215178124995832, -5.746835883940462963, 4.340624999385481964 ) ) ;
#4993 = CYLINDRICAL_SURFACE ( 'NONE', #8358, 0.5000000000000004441 ) ;
#4994 = CYLINDRICAL_SURFACE ( 'NONE', #14141, 4.000000000000000000 ) ;
#4995 = CARTESIAN_POINT ( 'NONE',  ( -23.46296185032722548, -19.82388608118403539, -6.500000000000000000 ) ) ;
#4996 = LINE ( 'NONE', #13113, #8830 ) ;
#4997 = CARTESIAN_POINT ( 'NONE',  ( -3.756430356249997438, -11.16877607737301048, 4.115624999385481431 ) ) ;
#4998 = CARTESIAN_POINT ( 'NONE',  ( 3.469446951953614189E-15, -8.999999999999992895, 0.000000000000000000 ) ) ;
#4999 = DIRECTION ( 'NONE',  ( 0.000000000000000000, 0.000000000000000000, 1.000000000000000000 ) ) ;
#5000 = ORIENTED_EDGE ( 'NONE', *, *, #17756, .F. ) ;
#5001 = ADVANCED_FACE ( 'NONE', ( #25813 ), #15505, .F. ) ;
#5002 = ORIENTED_EDGE ( 'NONE', *, *, #6339, .T. ) ;
#5003 = AXIS2_PLACEMENT_3D ( 'NONE', #232, #13965, #23760 ) ;
#5004 = ORIENTED_EDGE ( 'NONE', *, *, #6792, .T. ) ;
#5005 = CYLINDRICAL_SURFACE ( 'NONE', #3282, 4.000000000000000000 ) ;
#5006 = ORIENTED_EDGE ( 'NONE', *, *, #9966, .T. ) ;
#5007 = CARTESIAN_POINT ( 'NONE',  ( 3.756430356249996994, -25.47812499938548569, 8.999999999999992895 ) ) ;
#5008 = ORIENTED_EDGE ( 'NONE', *, *, #16401, .F. ) ;
#5009 = DIRECTION ( 'NONE',  ( -0.000000000000000000, -0.000000000000000000, 1.000000000000000000 ) ) ;
#5010 = AXIS2_PLACEMENT_3D ( 'NONE', #8397, #16387, #3032 ) ;
#5011 = CIRCLE ( 'NONE', #20432, 0.4999999999999998890 ) ;
#5012 = ORIENTED_EDGE ( 'NONE', *, *, #2940, .F. ) ;
#5013 = CARTESIAN_POINT ( 'NONE',  ( 1.999999999999995781, -29.19999999999999929, 5.535898384862237620 ) ) ;
#5014 = EDGE_CURVE ( 'NONE', #17574, #22373, #2481, .T. ) ;
#5015 = CARTESIAN_POINT ( 'NONE',  ( -3.756430356249995661, 29.37812499938548427, 6.831223922626973533 ) ) ;
#5016 = FACE_OUTER_BOUND ( 'NONE', #14044, .T. ) ;
#5017 = CARTESIAN_POINT ( 'NONE',  ( 7.734255490826784651, -30.12293631110048153, -6.500000000000000000 ) ) ;
#5018 = CARTESIAN_POINT ( 'NONE',  ( 18.09882730716638832, 19.61457683501836868, 12.99999999999999289 ) ) ;
#5019 = CARTESIAN_POINT ( 'NONE',  ( 17.37708538166121386, 20.03328275962052274, 12.25316411605951927 ) ) ;
#5020 = EDGE_CURVE ( 'NONE', #2753, #19084, #10301, .T. ) ;
#5021 = VECTOR ( 'NONE', #810, 1000.000000000000000 ) ;
#5022 = ADVANCED_FACE ( 'NONE', ( #21509 ), #1774, .T. ) ;
#5023 = CYLINDRICAL_SURFACE ( 'NONE', #19220, 31.10000000000000142 ) ;
#5024 = CARTESIAN_POINT ( 'NONE',  ( -1.878215178124998497, 29.49062499938548498, 12.25316411605951927 ) ) ;
#5025 = AXIS2_PLACEMENT_3D ( 'NONE', #16249, #566, #16124 ) ;
#5026 = CARTESIAN_POINT ( 'NONE',  ( 15.65123912826409480, 20.96363388418276941, 6.831223922626973533 ) ) ;
#5027 = LINE ( 'NONE', #17057, #15360 ) ;
#5028 = ORIENTED_EDGE ( 'NONE', *, *, #25754, .T. ) ;
#5029 = CARTESIAN_POINT ( 'NONE',  ( 8.012344526598182026E-15, 26.85624999877096997, 4.381197846482986158 ) ) ;
#5030 = CARTESIAN_POINT ( 'NONE',  ( 3.756430356249997438, -27.20312499938548356, 11.16877607737301048 ) ) ;
#5031 = CARTESIAN_POINT ( 'NONE',  ( 0.000000000000000000, 0.000000000000000000, 1.000000000000000000 ) ) ;
#5032 = AXIS2_PLACEMENT_3D ( 'NONE', #11971, #2046, #5706 ) ;
#5033 = CARTESIAN_POINT ( 'NONE',  ( 3.735045420075836212E-15, 25.36562499938548498, 4.662447845253954171 ) ) ;
#5034 = PLANE ( 'NONE',  #850 ) ;
#5036 = ORIENTED_EDGE ( 'NONE', *, *, #8279, .T. ) ;
#5035 = CYLINDRICAL_SURFACE ( 'NONE', #8275, 27.10000000000000142 ) ;
#5037 = ORIENTED_EDGE ( 'NONE', *, *, #6083, .F. ) ;
#5038 = PLANE ( 'NONE',  #9151 ) ;
#5039 = AXIS2_PLACEMENT_3D ( 'NONE', #10832, #9133, #658 ) ;
#5040 = VECTOR ( 'NONE', #16517, 1000.000000000000000 ) ;
#5041 = FACE_OUTER_BOUND ( 'NONE', #1236, .T. ) ;
#5042 = ORIENTED_EDGE ( 'NONE', *, *, #23060, .T. ) ;
#5043 = CLOSED_SHELL ( 'NONE', ( #18116, #11158, #25191, #1660, #25034, #8100, #19119, #5623, #10720, #24784, #12328, #16836, #6459, #2368, #1413, #20223, #10909, #15518, #12945, #13509, #13820, #19302, #16404, #4643, #6391, #22772, #24053, #23722, #8067, #4619, #15228, #10982, #21222, #3550, #5298, #25626, #1763, #5174, #5715, #14941, #22965, #11527, #22401, #16246, #18348, #13532, #18635, #15445, #8262, #17929, #8202, #23217, #17621, #24081, #18462, #17306, #20726, #11301, #20067, #17665, #15089, #4973, #7716, #25590, #456, #12540, #21190, #19855, #14841, #24192, #100, #679, #9935, #21455, #23886, #21314, #4243, #1282, #1539, #9431, #4460, #9797, #3887, #18134, #15371, #19192, #23963, #16731, #25151, #8046, #25237, #3200, #4534, #25086, #2697, #8499, #10471, #10960, #6092, #7467, #11741, #2112, #21458, #4280, #5056, #14112, #19326, #244, #16631, #4602, #25192, #17373, #15846, #22146, #19384, #21557, #3622, #22826, #4063, #7551, #16669, #7082, #25664, #944, #10570, #20719, #9652, #17118, #25427, #8463, #23511, #992, #22838, #890, #10404, #4396, #5022, #4015, #2523, #19782, #9532, #24831, #20215, #16066, #13765, #18589, #23838, #4743, #12402, #17577, #2871, #15810, #5366, #1032, #6746, #25787, #2190, #685, #5490, #21661, #736, #17113, #6646, #8236, #18054, #2471, #6967, #6128, #15737, #3486, #11386, #16038, #18598, #22292, #1102, #15559, #10159, #6466, #16601, #20413, #18019, #13025, #5756, #6429, #13489, #10244, #6488, #8055, #5414, #20473, #8132, #6365, #24023, #17667, #9927, #20376, #4980, #22670, #14176, #17193, #6944, #23951, #16508, #24394, #13731, #12012, #7391, #14602, #6991, #351, #10188, #9496, #3503, #17752, #24277, #22651, #1444, #8540, #23691, #7619, #894, #17699, #11046, #4001, #12283, #493, #13292, #12707, #12353, #12899, #22541, #15097, #12681, #18268, #14302, #9065, #1336, #20057, #7687, #8524, #20868, #16840, #17154, #25368, #14898, #21395, #13350, #10347, #8571, #22281, #1038, #22497, #25758, #15406, #11757, #13926 ) ) ;
#5044 = CYLINDRICAL_SURFACE ( 'NONE', #21856, 26.00000000000000711 ) ;
#5045 = CARTESIAN_POINT ( 'NONE',  ( -1.878215178124994722, 29.34062499938548640, 5.746835883940462963 ) ) ;
#5046 = CARTESIAN_POINT ( 'NONE',  ( 3.756430356250003211, 26.04062499938548925, 8.999999999999992895 ) ) ;
#5047 = AXIS2_PLACEMENT_3D ( 'NONE', #10443, #18437, #533 ) ;
#5048 = DIRECTION ( 'NONE',  ( 0.000000000000000000, 0.000000000000000000, 1.000000000000000000 ) ) ;
#5049 = CARTESIAN_POINT ( 'NONE',  ( 4.006172263299091013E-15, 28.17812499938548498, 13.33755215474602984 ) ) ;
#5050 = ADVANCED_FACE ( 'NONE', ( #3588 ), #25691, .T. ) ;
#5051 = ADVANCED_FACE ( 'NONE', ( #5679 ), #14322, .T. ) ;
#5052 = AXIS2_PLACEMENT_3D ( 'NONE', #24077, #9831, #4200 ) ;
#5053 = DIRECTION ( 'NONE',  ( 0.000000000000000000, -0.000000000000000000, 1.000000000000000000 ) ) ;
#5054 = DIRECTION ( 'NONE',  ( 1.000000000000000000, 0.000000000000000000, 0.000000000000000000 ) ) ;
#5055 = CARTESIAN_POINT ( 'NONE',  ( 3.959305671612554781E-15, 30.00000000000000355, 12.99999999999999289 ) ) ;
#5056 = ADVANCED_FACE ( 'NONE', ( #22542 ), #16414, .T. ) ;
#5057 = CIRCLE ( 'NONE', #1310, 0.5000000000000001110 ) ;
#5058 = CIRCLE ( 'NONE', #19646, 0.5000000000000001110 ) ;
#5059 = LINE ( 'NONE', #9368, #906 ) ;
#5060 = CARTESIAN_POINT ( 'NONE',  ( 3.756430356250003655, 27.39062499938548356, 8.999999999999992895 ) ) ;
#5061 = CARTESIAN_POINT ( 'NONE',  ( 16.23990935651709222, -26.52310962334749433, 1.000000000000000000 ) ) ;
#5062 = CARTESIAN_POINT ( 'NONE',  ( 21.91595456452976975, 19.25975718657032232, 12.25316411605952283 ) ) ;
#5063 = CARTESIAN_POINT ( 'NONE',  ( 17.58921741601718125, 20.24541479397648303, 5.746835883940462963 ) ) ;
#5064 = CARTESIAN_POINT ( 'NONE',  ( -16.66421332384646448, 26.25859848311288403, -6.500000000000000000 ) ) ;
#5065 = CARTESIAN_POINT ( 'NONE',  ( -3.756430356249997882, 29.00312499938548072, 11.16877607737301226 ) ) ;
#5066 = AXIS2_PLACEMENT_3D ( 'NONE', #9483, #8984, #11568 ) ;
#5067 = CARTESIAN_POINT ( 'NONE',  ( -26.25859848311247902, 16.66421332384710752, 1.000000000000000000 ) ) ;
#5068 = CARTESIAN_POINT ( 'NONE',  ( 22.05081056025715114, 16.73841580433833442, 6.831223922626973533 ) ) ;
#5069 = CARTESIAN_POINT ( 'NONE',  ( -1.999999999999998224, -12.46410161513774639, 2.999999999999999112 ) ) ;
#5070 = ORIENTED_EDGE ( 'NONE', *, *, #11892, .T. ) ;
#5071 = CARTESIAN_POINT ( 'NONE',  ( -11.44867358849371541, -28.91604871112453168, 1.000000000000000000 ) ) ;
#5072 = CARTESIAN_POINT ( 'NONE',  ( 3.752267015613588906E-15, 27.75624999877096855, 4.381197846482986158 ) ) ;
#5073 = CARTESIAN_POINT ( 'NONE',  ( -2.620986760973688460E-15, -25.33750000000000568, 13.61880215351699874 ) ) ;
#5075 = ORIENTED_EDGE ( 'NONE', *, *, #1169, .T. ) ;
#5074 = CARTESIAN_POINT ( 'NONE',  ( 4.000000000000003553, -8.999999999999992895, 3.543749998770967302 ) ) ;
#5076 = CARTESIAN_POINT ( 'NONE',  ( -1.878215178124995832, 27.20312499938548711, 5.746835883940462963 ) ) ;
#5077 = AXIS2_PLACEMENT_3D ( 'NONE', #22809, #9198, #8955 ) ;
#5078 = ORIENTED_EDGE ( 'NONE', *, *, #24234, .T. ) ;
#5079 = CARTESIAN_POINT ( 'NONE',  ( -3.756430356250002323, -29.15312499938548640, 11.16877607737301226 ) ) ;
#5080 = ORIENTED_EDGE ( 'NONE', *, *, #23723, .T. ) ;
#5081 = ORIENTED_EDGE ( 'NONE', *, *, #25543, .F. ) ;
#5082 = CARTESIAN_POINT ( 'NONE',  ( 19.26289903505010415, 22.99947435013303476, 12.01472878375390962 ) ) ;
#5083 = VECTOR ( 'NONE', #19050, 1000.000000000000000 ) ;
#5084 = CARTESIAN_POINT ( 'NONE',  ( 3.756430356250003211, 28.85312499938548569, 8.999999999999992895 ) ) ;
#5085 = AXIS2_PLACEMENT_3D ( 'NONE', #10028, #12121, #11866 ) ;
#5086 = CARTESIAN_POINT ( 'NONE',  ( 2.672651547586948120E-15, -13.33755215474603162, 1.378124999385482274 ) ) ;
#5087 = EDGE_CURVE ( 'NONE', #22637, #22373, #16146, .T. ) ;
#5088 = VECTOR ( 'NONE', #9520, 1000.000000000000000 ) ;
#5089 = EDGE_CURVE ( 'NONE', #19084, #22278, #7806, .T. ) ;
#5090 = CARTESIAN_POINT ( 'NONE',  ( -1.057460391440397258E-14, 29.10624999877096641, 4.999999999999992006 ) ) ;
#5091 = CARTESIAN_POINT ( 'NONE',  ( -1.071796769724491227, -27.28615380933863577, 4.999999999999989342 ) ) ;
#5092 = CARTESIAN_POINT ( 'NONE',  ( 1.878215178125004048, 29.26562499938548356, 5.746835883940462963 ) ) ;
#5093 = DIRECTION ( 'NONE',  ( 0.000000000000000000, 0.000000000000000000, 1.000000000000000000 ) ) ;
#5094 = AXIS2_PLACEMENT_3D ( 'NONE', #11723, #9768, #14441 ) ;
#5095 = DIRECTION ( 'NONE',  ( -0.000000000000000000, -0.000000000000000000, 1.000000000000000000 ) ) ;
#5096 = CARTESIAN_POINT ( 'NONE',  ( 2.672651547586948120E-15, 29.07812499938548356, 13.33755215474603162 ) ) ;
#5097 = FACE_OUTER_BOUND ( 'NONE', #762, .T. ) ;
#5098 = CARTESIAN_POINT ( 'NONE',  ( 3.999999999999976019, -11.30940107675851536, 0.8062499987709651483 ) ) ;
#5099 = CARTESIAN_POINT ( 'NONE',  ( 15.28676472490765548, 20.94361897439997122, 8.999999999999992895 ) ) ;
#5100 = CARTESIAN_POINT ( 'NONE',  ( 3.756430356249996994, -26.82812499938548711, 8.999999999999992895 ) ) ;
#5101 = AXIS2_PLACEMENT_3D ( 'NONE', #21971, #9812, #4046 ) ;
#5102 = CARTESIAN_POINT ( 'NONE',  ( -1.878215178124995832, 26.30312499938548498, 5.746835883940462963 ) ) ;
#5103 = CIRCLE ( 'NONE', #18047, 0.7500000000000001110 ) ;
#5105 = ADVANCED_FACE ( 'NONE', ( #18121 ), #16656, .F. ) ;
#5104 = PLANE ( 'NONE',  #11618 ) ;
#5106 = DIRECTION ( 'NONE',  ( 0.000000000000000000, -0.000000000000000000, -1.000000000000000000 ) ) ;
#5107 = DIRECTION ( 'NONE',  ( 0.000000000000000000, 0.000000000000000000, 1.000000000000000000 ) ) ;
#5108 = VERTEX_POINT ( 'NONE', #12738 ) ;
#5109 = CARTESIAN_POINT ( 'NONE',  ( -5.242581649506213637, 39.00274862415032118, 7.344859984781824558 ) ) ;
#5111 = ORIENTED_EDGE ( 'NONE', *, *, #13529, .F. ) ;
#5110 = DIRECTION ( 'NONE',  ( 1.000000000000000000, 0.000000000000000000, 0.000000000000000000 ) ) ;
#5112 =( BOUNDED_CURVE ( )  B_SPLINE_CURVE ( 2, ( #8075, #10656, #4393, #6487, #10149, #2567, #6222, #16565, #20337 ),
 .UNSPECIFIED., .F., .F. ) 
 B_SPLINE_CURVE_WITH_KNOTS ( ( 3, 2, 2, 2, 3 ),
 ( 0.7750000000000000222, 0.7833333333333333259, 0.8000000000000000444, 0.8166666666666666519, 0.8250000000000000666 ),
 .UNSPECIFIED. ) 
 CURVE ( )  GEOMETRIC_REPRESENTATION_ITEM ( )  RATIONAL_B_SPLINE_CURVE ( ( 0.9330127018922194093, 0.9330127018922194093, 1.000000000000000000, 0.8660254037844387076, 1.000000000000000000, 0.8660254037844387076, 1.000000000000000000, 0.9330127018922189652, 0.9330127018922194093 ) ) 
 REPRESENTATION_ITEM ( '' )  );
#5113 = AXIS2_PLACEMENT_3D ( 'NONE', #6363, #14082, #22047 ) ;
#5114 = ORIENTED_EDGE ( 'NONE', *, *, #15479, .F. ) ;
#5115 = VERTEX_POINT ( 'NONE', #4365 ) ;
#5116 = ORIENTED_EDGE ( 'NONE', *, *, #390, .F. ) ;
#5117 = ORIENTED_EDGE ( 'NONE', *, *, #21515, .T. ) ;
#5118 = CARTESIAN_POINT ( 'NONE',  ( -1.626862140677534194E-14, -27.58750000000000213, 12.99999999999999289 ) ) ;
#5119 =( BOUNDED_CURVE ( )  B_SPLINE_CURVE ( 2, ( #22478, #6650, #4557, #12541, #10965 ),
 .UNSPECIFIED., .F., .F. ) 
 B_SPLINE_CURVE_WITH_KNOTS ( ( 3, 2, 3 ),
 ( 0.9749999999999999778, 0.9833333333333332815, 0.9889400238386636399 ),
 .UNSPECIFIED. ) 
 CURVE ( )  GEOMETRIC_REPRESENTATION_ITEM ( )  RATIONAL_B_SPLINE_CURVE ( ( 0.9330127018922194093, 0.9330127018922194093, 1.000000000000000000, 0.9549307542065648136, 0.9401842259098239785 ) ) 
 REPRESENTATION_ITEM ( '' )  );
#5120 = LINE ( 'NONE', #3920, #5264 ) ;
#5121 = CIRCLE ( 'NONE', #20567, 31.10000000000000142 ) ;
#5122 = CARTESIAN_POINT ( 'NONE',  ( 3.735045420075836212E-15, 28.06562499938548427, 4.662447845253954171 ) ) ;
#5123 = CIRCLE ( 'NONE', #19725, 31.10000000000000142 ) ;
#5124 = AXIS2_PLACEMENT_3D ( 'NONE', #6023, #25514, #15976 ) ;
#5125 = CARTESIAN_POINT ( 'NONE',  ( -3.756430356249997882, -11.16877607737301226, 1.303124999385484095 ) ) ;
#5126 = CARTESIAN_POINT ( 'NONE',  ( 2.000000000000000888, -12.46410161513774817, 1.668749998770965970 ) ) ;
#5127 = CARTESIAN_POINT ( 'NONE',  ( 23.61528431363239022, 18.30288955771356640, 8.999999999999992895 ) ) ;
#5128 = CARTESIAN_POINT ( 'NONE',  ( 1.878215178125000939, 26.52812499938548285, 12.25316411605952283 ) ) ;
#5129 = CARTESIAN_POINT ( 'NONE',  ( 8.831537335106614961E-15, 26.23749999999999716, 12.99999999999999112 ) ) ;
#5131 = ADVANCED_FACE ( 'NONE', ( #590 ), #10357, .F. ) ;
#5130 = CARTESIAN_POINT ( 'NONE',  ( 3.735045420075836212E-15, -4.662447845253954171, 4.303124999385482319 ) ) ;
#5132 = CARTESIAN_POINT ( 'NONE',  ( 5.532151103383234236, 34.50000000000000000, 6.677220593914319657 ) ) ;
#5133 = DIRECTION ( 'NONE',  ( 0.000000000000000000, 0.000000000000000000, -1.000000000000000000 ) ) ;
#5134 = CARTESIAN_POINT ( 'NONE',  ( -1.071796769724492338, -29.40759618943233278, 12.99999999999999467 ) ) ;
#5135 = CARTESIAN_POINT ( 'NONE',  ( -1.071796769724489895, 29.76115380933864429, 12.99999999999999289 ) ) ;
#5136 = CARTESIAN_POINT ( 'NONE',  ( -3.756430356249997438, -11.16877607737301048, 3.665624999385481697 ) ) ;
#5137 = CARTESIAN_POINT ( 'NONE',  ( 3.137519842735244810E-15, -26.46249999999999858, 4.999999999999991118 ) ) ;
#5138 = CIRCLE ( 'NONE', #24753, 0.4999999999999998335 ) ;
#5139 = CARTESIAN_POINT ( 'NONE',  ( 17.08421000182778116, 25.98730014090436313, -6.500000000000000000 ) ) ;
#5140 = ORIENTED_EDGE ( 'NONE', *, *, #1839, .F. ) ;
#5141 = ORIENTED_EDGE ( 'NONE', *, *, #11265, .F. ) ;
#5142 = EDGE_CURVE ( 'NONE', #19442, #3077, #4486, .T. ) ;
#5143 = CIRCLE ( 'NONE', #22252, 31.10000000000000142 ) ;
#5144 = ORIENTED_EDGE ( 'NONE', *, *, #13139, .T. ) ;
#5145 = DIRECTION ( 'NONE',  ( 0.000000000000000000, 0.000000000000000000, 1.000000000000000000 ) ) ;
#5146 = ORIENTED_EDGE ( 'NONE', *, *, #24265, .T. ) ;
#5147 = FACE_OUTER_BOUND ( 'NONE', #22184, .T. ) ;
#5148 = VERTEX_POINT ( 'NONE', #10237 ) ;
#5149 = DIRECTION ( 'NONE',  ( 0.000000000000000000, 0.000000000000000000, 1.000000000000000000 ) ) ;
#5150 = CIRCLE ( 'NONE', #23508, 31.10000000000000142 ) ;
#5151 = EDGE_LOOP ( 'NONE', ( #9902, #23149, #17711, #4452 ) ) ;
#5152 = DIRECTION ( 'NONE',  ( -0.000000000000000000, -0.000000000000000000, -1.000000000000000000 ) ) ;
#5153 = CARTESIAN_POINT ( 'NONE',  ( 3.756430356250003655, 29.19062499938548072, 8.999999999999992895 ) ) ;
#5154 = CARTESIAN_POINT ( 'NONE',  ( 3.999999999999996447, -27.47499999999999787, 8.999999999999992895 ) ) ;
#5155 = CIRCLE ( 'NONE', #14742, 0.5000000000000000000 ) ;
#5156 = DIRECTION ( 'NONE',  ( 1.000000000000000000, 0.000000000000000000, 0.000000000000000000 ) ) ;
#5157 = CARTESIAN_POINT ( 'NONE',  ( 1.626862140677534194E-14, 28.43124999877096570, 12.99999999999999289 ) ) ;
#5158 = CARTESIAN_POINT ( 'NONE',  ( 16.60583328286593741, 21.91822803878461201, 6.831223922626973533 ) ) ;
#5159 = DIRECTION ( 'NONE',  ( 0.000000000000000000, 0.000000000000000000, 1.000000000000000000 ) ) ;
#5160 = CARTESIAN_POINT ( 'NONE',  ( 3.752267015613588906E-15, 26.46250000000000213, 4.381197846482986158 ) ) ;
#5161 = EDGE_CURVE ( 'NONE', #2304, #22503, #2533, .T. ) ;
#5162 = CARTESIAN_POINT ( 'NONE',  ( 17.37708538166121386, 20.03328275962052274, 12.25316411605951927 ) ) ;
#5163 = CARTESIAN_POINT ( 'NONE',  ( 3.469446951953614189E-15, -8.999999999999992895, 25.00000000000000000 ) ) ;
#5164 = ORIENTED_EDGE ( 'NONE', *, *, #10213, .T. ) ;
#5165 = CIRCLE ( 'NONE', #7254, 31.10000000000000142 ) ;
#5167 = EDGE_CURVE ( 'NONE', #12364, #22278, #194, .T. ) ;
#5166 = VERTEX_POINT ( 'NONE', #20434 ) ;
#5168 = CARTESIAN_POINT ( 'NONE',  ( -1.999999999999996669, 27.49374999877097636, 12.46410161513774639 ) ) ;
#5169 = CARTESIAN_POINT ( 'NONE',  ( 3.756430356249997438, -28.55312499938548498, 11.16877607737301048 ) ) ;
#5170 = CIRCLE ( 'NONE', #12250, 0.5000000000000002220 ) ;
#5171 = CARTESIAN_POINT ( 'NONE',  ( -14.98253926456298579, 27.25313774936435962, -6.500000000000000000 ) ) ;
#5172 = CARTESIAN_POINT ( 'NONE',  ( -3.756430356249997882, 27.76562499938549067, 11.16877607737301226 ) ) ;
#5173 = DIRECTION ( 'NONE',  ( 0.000000000000000000, 0.000000000000000000, 1.000000000000000000 ) ) ;
#5174 = ADVANCED_FACE ( 'NONE', ( #22682 ), #8167, .F. ) ;
#5175 = ORIENTED_EDGE ( 'NONE', *, *, #2268, .F. ) ;
#5176 = ORIENTED_EDGE ( 'NONE', *, *, #1162, .F. ) ;
#5177 = CARTESIAN_POINT ( 'NONE',  ( -27.25313774936430633, -14.98253926456308172, -6.500000000000000000 ) ) ;
#5178 = CARTESIAN_POINT ( 'NONE',  ( 3.469446951953614189E-15, -8.999999999999992895, 18.00000000000000000 ) ) ;
#5179 = ORIENTED_EDGE ( 'NONE', *, *, #11117, .T. ) ;
#5180 = CARTESIAN_POINT ( 'NONE',  ( 3.756430356249996994, -29.52812499938548640, 8.999999999999992895 ) ) ;
#5181 = CARTESIAN_POINT ( 'NONE',  ( 20.78451994863305430, 15.12766569914060888, 8.999999999999992895 ) ) ;
#5182 = LINE ( 'NONE', #12887, #11371 ) ;
#5183 =( GEOMETRIC_REPRESENTATION_CONTEXT ( 3 ) GLOBAL_UNCERTAINTY_ASSIGNED_CONTEXT ( ( #8895 ) ) GLOBAL_UNIT_ASSIGNED_CONTEXT ( ( #19711, #17117, #15166 ) ) REPRESENTATION_CONTEXT ( 'NONE', 'WORKASPACE' ) );
#5184 = DIRECTION ( 'NONE',  ( -0.7071067811865487940, -0.7071067811865463515, 0.000000000000000000 ) ) ;
#5185 = CARTESIAN_POINT ( 'NONE',  ( -3.999999999999996447, 25.22500000000000497, 8.999999999999992895 ) ) ;
#5186 = CARTESIAN_POINT ( 'NONE',  ( 30.85476721088025442, -3.897863563849982782, -6.500000000000000000 ) ) ;
#5187 = CARTESIAN_POINT ( 'NONE',  ( -3.999999999999996447, 27.02500000000000213, 8.999999999999992895 ) ) ;
#5188 = CARTESIAN_POINT ( 'NONE',  ( 4.000000000000003553, 29.69687499938548569, 8.999999999999992895 ) ) ;
#5189 = CARTESIAN_POINT ( 'NONE',  ( -3.756430356249997438, 27.20312499938548356, 11.16877607737301048 ) ) ;
#5190 = CARTESIAN_POINT ( 'NONE',  ( -1.999999999999994893, 26.89374999877097849, 5.535898384862237620 ) ) ;
#5191 = CARTESIAN_POINT ( 'NONE',  ( 16.47558800164659587, 19.30401512639272354, 12.46410161513774639 ) ) ;
#5192 = CARTESIAN_POINT ( 'NONE',  ( 19.61779375967526562, 22.44622088442137908, 12.46410161513774639 ) ) ;
#5193 = CARTESIAN_POINT ( 'NONE',  ( 20.14370442905180525, 20.14370442905174130, 12.99999999999999289 ) ) ;
#5194 = CARTESIAN_POINT ( 'NONE',  ( -3.756430356249997882, 28.55312499938548498, 11.16877607737301226 ) ) ;
#5195 = DIRECTION ( 'NONE',  ( 0.000000000000000000, 1.000000000000000000, 0.000000000000000000 ) ) ;
#5196 = CARTESIAN_POINT ( 'NONE',  ( 22.36900861179109867, 17.05661385587227841, 6.831223922626973533 ) ) ;
#5197 = CARTESIAN_POINT ( 'NONE',  ( -11.44867358849309547, 28.91604871112477326, -6.500000000000000000 ) ) ;
#5198 = EDGE_LOOP ( 'NONE', ( #22280, #15953, #21884, #8577 ) ) ;
#5199 = CARTESIAN_POINT ( 'NONE',  ( 3.469446951953614189E-15, -8.999999999999992895, 0.000000000000000000 ) ) ;
#5200 = CARTESIAN_POINT ( 'NONE',  ( -3.999999999999997335, 28.35624999877096997, 11.30940107675849404 ) ) ;
#5201 = CARTESIAN_POINT ( 'NONE',  ( -3.756430356250003655, -28.29062499938548569, 8.999999999999992895 ) ) ;
#5202 = EDGE_CURVE ( 'NONE', #1305, #14690, #1865, .T. ) ;
#5204 = ORIENTED_EDGE ( 'NONE', *, *, #10339, .T. ) ;
#5203 = CARTESIAN_POINT ( 'NONE',  ( 5.840899737312970963, 34.50000000000000000, 7.627451181685208859 ) ) ;
#5205 = CARTESIAN_POINT ( 'NONE',  ( -1.878215178124998497, 26.00312499938548783, 12.25316411605951927 ) ) ;
#5206 = EDGE_CURVE ( 'NONE', #25291, #24730, #1810, .T. ) ;
#5207 = ORIENTED_EDGE ( 'NONE', *, *, #11447, .T. ) ;
#5208 = CARTESIAN_POINT ( 'NONE',  ( 3.756430356249995661, -29.37812499938548427, 6.831223922626973533 ) ) ;
#5209 = VERTEX_POINT ( 'NONE', #6579 ) ;
#5210 = ORIENTED_EDGE ( 'NONE', *, *, #22674, .T. ) ;
#5211 = CARTESIAN_POINT ( 'NONE',  ( 21.21320343559646915, 21.21320343559638744, 12.99999999999999289 ) ) ;
#5212 = CARTESIAN_POINT ( 'NONE',  ( 1.878215178125008489, 28.92812499938549209, 5.746835883940462963 ) ) ;
#5213 = CARTESIAN_POINT ( 'NONE',  ( -3.756430356249996105, -6.831223922626973533, 1.678124999385481875 ) ) ;
#5214 = CARTESIAN_POINT ( 'NONE',  ( 2.672651547586948120E-15, -13.33755215474602984, 3.290624999385483918 ) ) ;
#5215 = DIRECTION ( 'NONE',  ( -1.000000000000000000, 0.000000000000000000, 0.000000000000000000 ) ) ;
#5216 = CARTESIAN_POINT ( 'NONE',  ( 4.000000000000000888, 28.63750000000000639, 6.690598923241489970 ) ) ;
#5217 = CARTESIAN_POINT ( 'NONE',  ( -2.899999999999996358, -8.999999999999992895, -10.00000000000000000 ) ) ;
#5218 = CARTESIAN_POINT ( 'NONE',  ( 3.735045420075836212E-15, 27.50312499938548427, 4.662447845253954171 ) ) ;
#5219 = DIRECTION ( 'NONE',  ( 0.000000000000000000, 0.000000000000000000, 1.000000000000000000 ) ) ;
#5220 = CARTESIAN_POINT ( 'NONE',  ( 7.901901826148023498E-15, 26.23750000000000426, 12.99999999999999112 ) ) ;
#5221 = CYLINDRICAL_SURFACE ( 'NONE', #6364, 0.5000000000000004441 ) ;
#5222 = DIRECTION ( 'NONE',  ( 0.4257792915650712717, -0.9048270524660203540, 0.000000000000000000 ) ) ;
#5223 = CARTESIAN_POINT ( 'NONE',  ( 3.756430356249996994, -28.62812499938548427, 8.999999999999992895 ) ) ;
#5224 = CARTESIAN_POINT ( 'NONE',  ( -27.25313774936430633, -14.98253926456308172, -6.500000000000000000 ) ) ;
#5225 = CARTESIAN_POINT ( 'NONE',  ( -10.98232076577180649, 29.09636799667095630, -2.750000000000000000 ) ) ;
#5226 = CARTESIAN_POINT ( 'NONE',  ( -1.071796769724488563, 26.16115380933863221, 12.99999999999999289 ) ) ;
#5227 = EDGE_CURVE ( 'NONE', #21732, #7703, #11826, .T. ) ;
#5228 = CARTESIAN_POINT ( 'NONE',  ( 23.07819757097597702, 17.42134332148352627, 6.690598923241489970 ) ) ;
#5229 = EDGE_LOOP ( 'NONE', ( #23264, #6089, #12306, #16444 ) ) ;
#5230 = CARTESIAN_POINT ( 'NONE',  ( 3.756430356250003655, 29.69687499938548569, 8.999999999999992895 ) ) ;
#5232 = ORIENTED_EDGE ( 'NONE', *, *, #18103, .F. ) ;
#5231 = DIRECTION ( 'NONE',  ( 0.6374239897486886353, -0.7705132427757902525, 0.000000000000000000 ) ) ;
#5233 = EDGE_CURVE ( 'NONE', #5209, #1087, #7239, .T. ) ;
#5234 = ORIENTED_EDGE ( 'NONE', *, *, #2985, .T. ) ;
#5235 = ORIENTED_EDGE ( 'NONE', *, *, #24881, .F. ) ;
#5236 = ORIENTED_EDGE ( 'NONE', *, *, #11312, .F. ) ;
#5237 = ORIENTED_EDGE ( 'NONE', *, *, #7530, .T. ) ;
#5238 = CYLINDRICAL_SURFACE ( 'NONE', #13046, 4.000000000000000000 ) ;
#5239 = DIRECTION ( 'NONE',  ( 0.000000000000000000, 0.000000000000000000, 1.000000000000000000 ) ) ;
#5240 = CARTESIAN_POINT ( 'NONE',  ( 23.36385188462466900, 18.81896140916762050, 11.39306173506717457 ) ) ;
#5241 = EDGE_CURVE ( 'NONE', #20109, #6572, #8913, .T. ) ;
#5242 = CARTESIAN_POINT ( 'NONE',  ( 2.672651547586948120E-15, -13.33755215474602984, 0.9281249993854824298 ) ) ;
#5243 = CARTESIAN_POINT ( 'NONE',  ( 2.000000000000000888, -12.46410161513774817, 2.568749998770967213 ) ) ;
#5244 = CARTESIAN_POINT ( 'NONE',  ( 20.08404229395466700, 20.08404229395459240, 4.662447845253954171 ) ) ;
#5245 = CARTESIAN_POINT ( 'NONE',  ( 3.756430356250003655, 26.60312499938548569, 8.999999999999992895 ) ) ;
#5246 = CARTESIAN_POINT ( 'NONE',  ( 3.469446951953614189E-15, 38.49999999999999289, 8.999999999999992895 ) ) ;
#5247 = CARTESIAN_POINT ( 'NONE',  ( 3.469446951953614189E-15, 39.50000000000000000, 8.999999999999992895 ) ) ;
#5248 = CARTESIAN_POINT ( 'NONE',  ( -1.999999999999995781, -5.535898384862237620, 0.5999999999999998668 ) ) ;
#5249 = DIRECTION ( 'NONE',  ( 0.000000000000000000, -0.000000000000000000, 1.000000000000000000 ) ) ;
#5250 = CARTESIAN_POINT ( 'NONE',  ( 18.55271417138208179, 18.55271417138200363, 12.99999999999999112 ) ) ;
#5251 = CARTESIAN_POINT ( 'NONE',  ( 17.54066758993977970, 23.19752183943208479, 11.30940107675849404 ) ) ;
#5252 =( BOUNDED_CURVE ( )  B_SPLINE_CURVE ( 2, ( #10255, #10644, #12231, #24641, #22421, #4781, #10769 ),
 .UNSPECIFIED., .F., .F. ) 
 B_SPLINE_CURVE_WITH_KNOTS ( ( 3, 2, 2, 3 ),
 ( 0.04999999999999990563, 0.06666666666666654084, 0.08333333333333316217, 0.09999999999999981126 ),
 .UNSPECIFIED. ) 
 CURVE ( )  GEOMETRIC_REPRESENTATION_ITEM ( )  RATIONAL_B_SPLINE_CURVE ( ( 1.000000000000000666, 0.8660254037844378194, 1.000000000000000000, 0.8660254037844387076, 1.000000000000000000, 0.8660254037844402619, 0.9999999999999984457 ) ) 
 REPRESENTATION_ITEM ( '' )  );
#5253 = CARTESIAN_POINT ( 'NONE',  ( -3.752267015613588906E-15, -25.95624999877096784, 4.381197846482986158 ) ) ;
#5254 = CYLINDRICAL_SURFACE ( 'NONE', #24252, 4.000000000000000000 ) ;
#5255 = CYLINDRICAL_SURFACE ( 'NONE', #17879, 0.5000000000000004441 ) ;
#5256 = CARTESIAN_POINT ( 'NONE',  ( -1.071796769724488563, 25.76740381056766793, 12.99999999999999289 ) ) ;
#5257 = ORIENTED_EDGE ( 'NONE', *, *, #9458, .T. ) ;
#5258 = CARTESIAN_POINT ( 'NONE',  ( -25.99307600111999150, 0.5999999999999998668, 19.00000000000000000 ) ) ;
#5259 = ORIENTED_EDGE ( 'NONE', *, *, #9136, .F. ) ;
#5260 =( BOUNDED_CURVE ( )  B_SPLINE_CURVE ( 2, ( #2575, #8983, #18540, #10398, #10790, #20477, #22842, #22320, #22443 ),
 .UNSPECIFIED., .F., .F. ) 
 B_SPLINE_CURVE_WITH_KNOTS ( ( 3, 2, 2, 2, 3 ),
 ( 0.7249999999999999778, 0.7333333333333332815, 0.7500000000000000000, 0.7666666666666667185, 0.7750000000000000222 ),
 .UNSPECIFIED. ) 
 CURVE ( )  GEOMETRIC_REPRESENTATION_ITEM ( )  RATIONAL_B_SPLINE_CURVE ( ( 0.9330127018922194093, 0.9330127018922194093, 1.000000000000000000, 0.8660254037844387076, 1.000000000000000000, 0.8660254037844387076, 1.000000000000000000, 0.9330127018922194093, 0.9330127018922194093 ) ) 
 REPRESENTATION_ITEM ( '' )  );
#5261 = ORIENTED_EDGE ( 'NONE', *, *, #12763, .F. ) ;
#5262 = DIRECTION ( 'NONE',  ( -0.000000000000000000, -0.000000000000000000, -1.000000000000000000 ) ) ;
#5263 = VERTEX_POINT ( 'NONE', #11142 ) ;
#5264 = VECTOR ( 'NONE', #9679, 1000.000000000000000 ) ;
#5265 = CARTESIAN_POINT ( 'NONE',  ( 9.610428525060671134, -29.57785765677934009, -6.500000000000000000 ) ) ;
#5266 = ORIENTED_EDGE ( 'NONE', *, *, #10513, .F. ) ;
#5267 = LINE ( 'NONE', #23304, #13034 ) ;
#5268 = EDGE_CURVE ( 'NONE', #18492, #15884, #23510, .T. ) ;
#5269 = EDGE_LOOP ( 'NONE', ( #15348, #17520, #22173, #9888, #19145 ) ) ;
#5270 = CARTESIAN_POINT ( 'NONE',  ( 4.000000000000003553, 27.25000000000000000, 8.999999999999992895 ) ) ;
#5271 = DIRECTION ( 'NONE',  ( -0.000000000000000000, -0.000000000000000000, 1.000000000000000000 ) ) ;
#5272 = ADVANCED_FACE ( 'NONE', ( #9680 ), #13723, .T. ) ;
#5273 = CARTESIAN_POINT ( 'NONE',  ( 1.071796769724491227, 26.44240381056766509, 4.999999999999989342 ) ) ;
#5274 = DIRECTION ( 'NONE',  ( 0.1873813145857330109, 0.9822872507286871668, 0.000000000000000000 ) ) ;
#5275 = CARTESIAN_POINT ( 'NONE',  ( 21.49396397007274473, 16.18156921415393157, 6.831223922626973533 ) ) ;
#5276 = LINE ( 'NONE', #11281, #7942 ) ;
#5277 = CIRCLE ( 'NONE', #696, 30.00000000000000355 ) ;
#5278 = CARTESIAN_POINT ( 'NONE',  ( 2.620986760973688460E-15, 26.68750000000000000, 13.61880215351699874 ) ) ;
#5279 = CARTESIAN_POINT ( 'NONE',  ( 19.04989862646933929, 19.04989862646927534, 13.33755215474603162 ) ) ;
#5280 = DIRECTION ( 'NONE',  ( 1.000000000000000000, 0.000000000000000000, 0.000000000000000000 ) ) ;
#5281 = EDGE_LOOP ( 'NONE', ( #17331, #17655, #14630, #10678 ) ) ;
#5282 = ORIENTED_EDGE ( 'NONE', *, *, #11200, .T. ) ;
#5283 = CARTESIAN_POINT ( 'NONE',  ( 6.009258394948636914E-15, 28.20624999877096784, 4.381197846482986158 ) ) ;
#5284 = LINE ( 'NONE', #11910, #2053 ) ;
#5285 = VERTEX_POINT ( 'NONE', #15574 ) ;
#5286 = CARTESIAN_POINT ( 'NONE',  ( -30.60000000000000142, 3.257552089140643357E-13, -6.500000000000000000 ) ) ;
#5287 = CARTESIAN_POINT ( 'NONE',  ( 3.756430356250004099, 27.99062499938548498, 6.831223922626973533 ) ) ;
#5288 = DIRECTION ( 'NONE',  ( -0.000000000000000000, -1.000000000000000000, -0.000000000000000000 ) ) ;
#5289 = ORIENTED_EDGE ( 'NONE', *, *, #15336, .T. ) ;
#5290 = VERTEX_POINT ( 'NONE', #21098 ) ;
#5291 = CARTESIAN_POINT ( 'NONE',  ( 0.000000000000000000, 0.000000000000000000, -6.500000000000000000 ) ) ;
#5292 = EDGE_CURVE ( 'NONE', #16864, #284, #17044, .T. ) ;
#5293 = DIRECTION ( 'NONE',  ( 0.000000000000000000, -1.000000000000000000, 0.000000000000000000 ) ) ;
#5294 = VERTEX_POINT ( 'NONE', #19121 ) ;
#5295 = CARTESIAN_POINT ( 'NONE',  ( -3.735045420075836212E-15, -28.51562499938548356, 4.662447845253954171 ) ) ;
#5296 = CARTESIAN_POINT ( 'NONE',  ( -1.878215178124998275, 29.49062499938548854, 12.25316411605951927 ) ) ;
#5297 = CARTESIAN_POINT ( 'NONE',  ( -1.878215178124996498, 26.19062499938548783, 5.746835883940462963 ) ) ;
#5298 = ADVANCED_FACE ( 'NONE', ( #1213 ), #18883, .F. ) ;
#5299 = CARTESIAN_POINT ( 'NONE',  ( 3.469446951953614189E-15, 31.50000000000000000, 8.999999999999992895 ) ) ;
#5300 = CARTESIAN_POINT ( 'NONE',  ( 3.756430356250002323, 29.60312499938548925, 11.16877607737301226 ) ) ;
#5301 = EDGE_CURVE ( 'NONE', #9082, #16618, #18517, .T. ) ;
#5302 = CARTESIAN_POINT ( 'NONE',  ( 4.000000000000005329, 25.41250000000000497, 11.30940107675849760 ) ) ;
#5303 = APPLICATION_PROTOCOL_DEFINITION ( 'draft international standard', 'automotive_design', 1998, #8614 ) ;
#5304 = EDGE_CURVE ( 'NONE', #7798, #8491, #22805, .T. ) ;
#5305 = CARTESIAN_POINT ( 'NONE',  ( -3.999999999999997335, 27.06250000000000000, 11.30940107675849404 ) ) ;
#5306 = CARTESIAN_POINT ( 'NONE',  ( -8.831537335106614961E-15, -27.13750000000000284, 12.99999999999999112 ) ) ;
#5307 = CARTESIAN_POINT ( 'NONE',  ( 2.672651547586948120E-15, 25.92812499938548498, 13.33755215474603162 ) ) ;
#5308 = DIRECTION ( 'NONE',  ( 1.000000000000000000, 0.000000000000000000, -0.000000000000000000 ) ) ;
#5309 = CARTESIAN_POINT ( 'NONE',  ( 20.24314131972164432, 20.24314131972156972, 13.33755215474602984 ) ) ;
#5310 = CARTESIAN_POINT ( 'NONE',  ( 20.82877788845545552, 18.17258051049600454, 5.746835883940462963 ) ) ;
#5311 = DIRECTION ( 'NONE',  ( 0.8443279255020205154, 0.5358267949789882190, 0.000000000000000000 ) ) ;
#5312 = CARTESIAN_POINT ( 'NONE',  ( -3.756430356249995661, 28.47812499938548569, 6.831223922626973533 ) ) ;
#5313 = CARTESIAN_POINT ( 'NONE',  ( 22.43212701321220948, 19.92128553278266878, 5.406171146378998316 ) ) ;
#5314 = CARTESIAN_POINT ( 'NONE',  ( 17.61573392031167273, 20.27193129827097806, 12.25316411605951927 ) ) ;
#5315 = CARTESIAN_POINT ( 'NONE',  ( 4.000000000000032863, -11.30940107675847983, 3.112500000000002487 ) ) ;
#5316 = ORIENTED_EDGE ( 'NONE', *, *, #22898, .F. ) ;
#5317 = CARTESIAN_POINT ( 'NONE',  ( 18.71181319714904490, 18.71181319714897384, 4.999999999999991118 ) ) ;
#5318 = CARTESIAN_POINT ( 'NONE',  ( -1.878215178124998497, 26.45312499938548711, 12.25316411605951927 ) ) ;
#5319 = CARTESIAN_POINT ( 'NONE',  ( -2.672651547586948120E-15, -29.52812499938548285, 13.33755215474602984 ) ) ;
#5321 = VERTEX_POINT ( 'NONE', #23542 ) ;
#5320 = CARTESIAN_POINT ( 'NONE',  ( -3.999999999999997335, 25.26249999999999929, 11.30940107675849404 ) ) ;
#5322 = CARTESIAN_POINT ( 'NONE',  ( 3.735045420075836212E-15, 25.81562499938548783, 4.662447845253954171 ) ) ;
#5323 = CARTESIAN_POINT ( 'NONE',  ( -19.58805710660148236, 17.18149551509898743, 20.00001200000000523 ) ) ;
#5324 = CARTESIAN_POINT ( 'NONE',  ( 3.756430356249995661, -27.12812499938548427, 6.831223922626973533 ) ) ;
#5325 = ORIENTED_EDGE ( 'NONE', *, *, #4522, .F. ) ;
#5326 = ORIENTED_EDGE ( 'NONE', *, *, #2230, .F. ) ;
#5327 = CARTESIAN_POINT ( 'NONE',  ( 18.29810693902837571, 23.77355554533980353, 10.03836643961819419 ) ) ;
#5328 = CARTESIAN_POINT ( 'NONE',  ( -3.756430356249996549, 27.27812499938548996, 8.999999999999992895 ) ) ;
#5329 = CARTESIAN_POINT ( 'NONE',  ( 3.756430356250003211, -6.831223922626973533, 1.978124999385481919 ) ) ;
#5330 = EDGE_CURVE ( 'NONE', #27, #7696, #7241, .T. ) ;
#5331 = AXIS2_PLACEMENT_3D ( 'NONE', #15487, #4891, #8961 ) ;
#5332 = CARTESIAN_POINT ( 'NONE',  ( -3.756430356249996994, -8.999999999999992895, 4.078124999385482674 ) ) ;
#5333 = PRESENTATION_STYLE_ASSIGNMENT (( #17631 ) ) ;
#5334 = EDGE_CURVE ( 'NONE', #7544, #17713, #21548, .T. ) ;
#5335 = CARTESIAN_POINT ( 'NONE',  ( 0.000000000000000000, 0.000000000000000000, -6.500000000000000000 ) ) ;
#5336 = EDGE_CURVE ( 'NONE', #4455, #12921, #13606, .T. ) ;
#5337 = CARTESIAN_POINT ( 'NONE',  ( 26.52310962334750855, 16.23990935651707801, -2.750000000000000000 ) ) ;
#5338 = DIRECTION ( 'NONE',  ( 1.000000000000000000, 0.000000000000000000, 0.000000000000000000 ) ) ;
#5339 = CARTESIAN_POINT ( 'NONE',  ( 0.000000000000000000, 0.000000000000000000, -6.500000000000000000 ) ) ;
#5340 = DIRECTION ( 'NONE',  ( -0.000000000000000000, 1.000000000000000000, 0.000000000000000000 ) ) ;
#5341 = DIRECTION ( 'NONE',  ( -0.000000000000000000, 0.000000000000000000, 1.000000000000000000 ) ) ;
#5342 = CARTESIAN_POINT ( 'NONE',  ( 3.878215178125003604, 25.07031249969274356, 8.999999999999992895 ) ) ;
#5343 = CARTESIAN_POINT ( 'NONE',  ( 5.797192864167126203, 38.54534174146481718, 7.639664215341221976 ) ) ;
#5344 = CARTESIAN_POINT ( 'NONE',  ( -3.756430356250002323, -28.36562499938548854, 11.16877607737301226 ) ) ;
#5345 = CARTESIAN_POINT ( 'NONE',  ( 17.22246953840583572, 22.87932378789814436, 11.30940107675849404 ) ) ;
#5346 = DIRECTION ( 'NONE',  ( -0.7071067811865487940, -0.7071067811865463515, 0.000000000000000000 ) ) ;
#5347 = DIRECTION ( 'NONE',  ( 0.000000000000000000, 0.000000000000000000, 1.000000000000000000 ) ) ;
#5348 = ORIENTED_EDGE ( 'NONE', *, *, #25333, .F. ) ;
#5349 = CARTESIAN_POINT ( 'NONE',  ( 4.000000000000003553, 27.25000000000000000, 8.999999999999992895 ) ) ;
#5350 = LINE ( 'NONE', #24854, #10861 ) ;
#5352 = ORIENTED_EDGE ( 'NONE', *, *, #4988, .T. ) ;
#5351 = CARTESIAN_POINT ( 'NONE',  ( 18.23451611984813425, 18.23451611984805609, 12.99999999999999112 ) ) ;
#5353 = ORIENTED_EDGE ( 'NONE', *, *, #13246, .T. ) ;
#5354 = AXIS2_PLACEMENT_3D ( 'NONE', #15715, #7992, #5641 ) ;
#5355 = VERTEX_POINT ( 'NONE', #23664 ) ;
#5356 = ORIENTED_EDGE ( 'NONE', *, *, #7759, .T. ) ;
#5357 = ORIENTED_EDGE ( 'NONE', *, *, #10784, .T. ) ;
#5358 = CARTESIAN_POINT ( 'NONE',  ( 0.000000000000000000, 0.000000000000000000, 1.000000000000000000 ) ) ;
#5359 = CARTESIAN_POINT ( 'NONE',  ( -1.057460391440397258E-14, 29.10624999877096641, 4.999999999999992006 ) ) ;
#5360 = VECTOR ( 'NONE', #21334, 1000.000000000000114 ) ;
#5361 = CARTESIAN_POINT ( 'NONE',  ( -1.999999999999994893, 27.85000000000000497, 5.535898384862237620 ) ) ;
#5362 = CARTESIAN_POINT ( 'NONE',  ( -1.878215178124998497, -12.25316411605951927, 0.8906249993854836733 ) ) ;
#5363 = CARTESIAN_POINT ( 'NONE',  ( -3.999999999999996003, -6.690598923241487306, 2.831249998770966059 ) ) ;
#5364 =( NAMED_UNIT ( * ) SI_UNIT ( $, .STERADIAN. ) SOLID_ANGLE_UNIT ( ) );
#5365 = CARTESIAN_POINT ( 'NONE',  ( -3.756430356249997882, 25.96562499938548640, 11.16877607737301226 ) ) ;
#5366 = ADVANCED_FACE ( 'NONE', ( #831 ), #2788, .F. ) ;
#5367 = DIRECTION ( 'NONE',  ( 0.000000000000000000, -1.000000000000000000, 0.000000000000000000 ) ) ;
#5368 = CYLINDRICAL_SURFACE ( 'NONE', #16811, 4.000000000000000000 ) ;
#5369 = CARTESIAN_POINT ( 'NONE',  ( -3.999999999999996447, -8.999999999999992895, 1.574999999999999956 ) ) ;
#5370 = VECTOR ( 'NONE', #13168, 1000.000000000000114 ) ;
#5371 = CYLINDRICAL_SURFACE ( 'NONE', #21726, 4.000000000000000000 ) ;
#5372 = DIRECTION ( 'NONE',  ( 0.000000000000000000, 0.000000000000000000, -1.000000000000000000 ) ) ;
#5373 = DIRECTION ( 'NONE',  ( 0.000000000000000000, 0.000000000000000000, 1.000000000000000000 ) ) ;
#5374 = CARTESIAN_POINT ( 'NONE',  ( -2.620986760973688460E-15, -27.98124999877096997, 13.61880215351699874 ) ) ;
#5375 = ADVANCED_FACE ( 'NONE', ( #19602 ), #20179, .T. ) ;
#5376 = CARTESIAN_POINT ( 'NONE',  ( 3.756430356250002323, -11.16877607737301403, 3.365624999385485872 ) ) ;
#5377 = VECTOR ( 'NONE', #25776, 999.9999999999998863 ) ;
#5378 = CARTESIAN_POINT ( 'NONE',  ( 1.999999999999998224, -26.64999999999999858, 12.46410161513774639 ) ) ;
#5380 = CIRCLE ( 'NONE', #19982, 2.899999999999999911 ) ;
#5379 = DIRECTION ( 'NONE',  ( 0.000000000000000000, 0.000000000000000000, 1.000000000000000000 ) ) ;
#5381 = CARTESIAN_POINT ( 'NONE',  ( -4.000000000000003553, -25.93750000000000000, 6.690598923241489970 ) ) ;
#5382 = VERTEX_POINT ( 'NONE', #22927 ) ;
#5383 = CARTESIAN_POINT ( 'NONE',  ( 3.469446951953614189E-15, -8.999999999999992895, 18.00000000000000000 ) ) ;
#5384 = ORIENTED_EDGE ( 'NONE', *, *, #5233, .F. ) ;
#5385 = VERTEX_POINT ( 'NONE', #3056 ) ;
#5386 = CARTESIAN_POINT ( 'NONE',  ( 0.000000000000000000, 0.000000000000000000, 17.00000000000000000 ) ) ;
#5387 = VERTEX_POINT ( 'NONE', #19005 ) ;
#5388 = CARTESIAN_POINT ( 'NONE',  ( 3.756430356249995661, -27.24062499938548498, 6.831223922626973533 ) ) ;
#5389 = ORIENTED_EDGE ( 'NONE', *, *, #11775, .T. ) ;
#5390 = EDGE_LOOP ( 'NONE', ( #22334, #6903, #8523, #24492 ) ) ;
#5391 = CARTESIAN_POINT ( 'NONE',  ( 2.000000000000003997, 27.77500000000000213, 5.535898384862238508 ) ) ;
#5392 = CARTESIAN_POINT ( 'NONE',  ( 5.827558883616049457, 30.54913349766221842, -6.500000000000000000 ) ) ;
#5393 = VECTOR ( 'NONE', #23364, 1000.000000000000000 ) ;
#5394 = MANIFOLD_SOLID_BREP ( 'Cavity1', #10872 ) ;
#5395 = AXIS2_PLACEMENT_3D ( 'NONE', #8906, #14788, #8633 ) ;
#5396 = CARTESIAN_POINT ( 'NONE',  ( 8.831537335106614961E-15, 26.23749999999999716, 12.99999999999999112 ) ) ;
#5397 = DIRECTION ( 'NONE',  ( 0.000000000000000000, 0.000000000000000000, 1.000000000000000000 ) ) ;
#5398 = CARTESIAN_POINT ( 'NONE',  ( 18.19682354053567153, 23.50921829645433903, 6.831223922626973533 ) ) ;
#5399 = EDGE_CURVE ( 'NONE', #17170, #4613, #14356, .T. ) ;
#5400 =( BOUNDED_CURVE ( )  B_SPLINE_CURVE ( 2, ( #23965, #6046, #16244, #14029, #12045, #22260, #4341, #19779, #10334 ),
 .UNSPECIFIED., .F., .F. ) 
 B_SPLINE_CURVE_WITH_KNOTS ( ( 3, 2, 2, 2, 3 ),
 ( 0.1749999999999999889, 0.1833333333333333204, 0.2000000000000000111, 0.2166666666666666741, 0.2250000000000000056 ),
 .UNSPECIFIED. ) 
 CURVE ( )  GEOMETRIC_REPRESENTATION_ITEM ( )  RATIONAL_B_SPLINE_CURVE ( ( 0.9330127018922194093, 0.9330127018922194093, 1.000000000000000000, 0.8660254037844387076, 1.000000000000000000, 0.8660254037844387076, 1.000000000000000000, 0.9330127018922194093, 0.9330127018922194093 ) ) 
 REPRESENTATION_ITEM ( '' )  );
#5401 = DIRECTION ( 'NONE',  ( -0.000000000000000000, -0.000000000000000000, 1.000000000000000000 ) ) ;
#5402 = EDGE_CURVE ( 'NONE', #20971, #12396, #4880, .T. ) ;
#5403 = CARTESIAN_POINT ( 'NONE',  ( 2.000000000000000888, 25.82499999999999929, 12.46410161513774817 ) ) ;
#5404 =( BOUNDED_CURVE ( )  B_SPLINE_CURVE ( 2, ( #17429, #7743, #25277, #15470, #1739, #17180, #19118, #5527, #3558 ),
 .UNSPECIFIED., .F., .F. ) 
 B_SPLINE_CURVE_WITH_KNOTS ( ( 3, 2, 2, 2, 3 ),
 ( 0.8250000000000000666, 0.8333333333333333703, 0.8499999999999999778, 0.8666666666666666963, 0.8750000000000000000 ),
 .UNSPECIFIED. ) 
 CURVE ( )  GEOMETRIC_REPRESENTATION_ITEM ( )  RATIONAL_B_SPLINE_CURVE ( ( 0.9330127018922194093, 0.9330127018922198534, 1.000000000000000000, 0.8660254037844387076, 1.000000000000000000, 0.8660254037844387076, 1.000000000000000000, 0.9330127018922194093, 0.9330127018922194093 ) ) 
 REPRESENTATION_ITEM ( '' )  );
#5405=STYLED_ITEM('',(#25907),#13235);
#5406 = CARTESIAN_POINT ( 'NONE',  ( 22.42204162038009230, 17.10964686446126848, 8.999999999999992895 ) ) ;
#5407 = CARTESIAN_POINT ( 'NONE',  ( 4.081770351527290718E-15, 39.50000000000000000, 13.99999999999999289 ) ) ;
#5408 = AXIS2_PLACEMENT_3D ( 'NONE', #18969, #19086, #5110 ) ;
#5409 = VERTEX_POINT ( 'NONE', #12282 ) ;
#5410 = VERTEX_POINT ( 'NONE', #5878 ) ;
#5411 = CARTESIAN_POINT ( 'NONE',  ( -3.999999999999996447, 28.80624999877096926, 11.30940107675849404 ) ) ;
#5413 = CARTESIAN_POINT ( 'NONE',  ( 21.21320343559646915, 21.21320343559638744, 12.99999999999999289 ) ) ;
#5412 = VECTOR ( 'NONE', #9336, 1000.000000000000000 ) ;
#5414 = ADVANCED_FACE ( 'NONE', ( #18296 ), #7835, .F. ) ;
#5415 = ORIENTED_EDGE ( 'NONE', *, *, #9720, .T. ) ;
#5416 = CARTESIAN_POINT ( 'NONE',  ( 19.50730832598392084, 19.50730832598383913, 12.99999999999999289 ) ) ;
#5417 = AXIS2_PLACEMENT_3D ( 'NONE', #17332, #19276, #17062 ) ;
#5418 = CARTESIAN_POINT ( 'NONE',  ( -1.878215178124998497, 28.25312499938548427, 12.25316411605951927 ) ) ;
#5419 = DIRECTION ( 'NONE',  ( 0.000000000000000000, 0.000000000000000000, 1.000000000000000000 ) ) ;
#5420 = ORIENTED_EDGE ( 'NONE', *, *, #18266, .F. ) ;
#5421 = ORIENTED_EDGE ( 'NONE', *, *, #25545, .T. ) ;
#5422 = CYLINDRICAL_SURFACE ( 'NONE', #7466, 4.000000000000000000 ) ;
#5423 = CARTESIAN_POINT ( 'NONE',  ( -12.78762572734017589, 28.34936733434218681, -2.750000000000000000 ) ) ;
#5424 = AXIS2_PLACEMENT_3D ( 'NONE', #16226, #3671, #11649 ) ;
#5425 = ORIENTED_EDGE ( 'NONE', *, *, #8327, .F. ) ;
#5426 = CARTESIAN_POINT ( 'NONE',  ( 1.626862140677534194E-14, 28.43124999877096570, 12.99999999999999289 ) ) ;
#5427 = CARTESIAN_POINT ( 'NONE',  ( -3.756430356249996549, 28.92812499938548854, 6.831223922626973533 ) ) ;
#5428 = AXIS2_PLACEMENT_3D ( 'NONE', #14934, #16777, #25132 ) ;
#5429 = DIRECTION ( 'NONE',  ( 1.000000000000000000, 0.000000000000000000, 0.000000000000000000 ) ) ;
#5430 = CARTESIAN_POINT ( 'NONE',  ( 2.000000000000007105, 26.87500000000001066, 5.535898384862238508 ) ) ;
#5431 = APPLICATION_PROTOCOL_DEFINITION ( 'draft international standard', 'automotive_design', 1998, #10427 ) ;
#5432 = DIRECTION ( 'NONE',  ( -1.000000000000000000, 0.000000000000000000, 0.000000000000000000 ) ) ;
#5433 = DIRECTION ( 'NONE',  ( -0.000000000000000000, -0.000000000000000000, 1.000000000000000000 ) ) ;
#5434 = CARTESIAN_POINT ( 'NONE',  ( 3.756430356250002323, 26.00312499938548427, 11.16877607737301403 ) ) ;
#5435 = MANIFOLD_SOLID_BREP ( 'Extrude-Thin1', #13391 ) ;
#5436 = AXIS2_PLACEMENT_3D ( 'NONE', #18762, #1234, #21114 ) ;
#5437 = LINE ( 'NONE', #5690, #21666 ) ;
#5438 = CARTESIAN_POINT ( 'NONE',  ( 18.17030703624117294, 23.48270179215984754, 11.16877607737301226 ) ) ;
#5439 = CARTESIAN_POINT ( 'NONE',  ( 19.52719570377026415, 19.52719570377018599, 4.662447845253954171 ) ) ;
#5440 = CARTESIAN_POINT ( 'NONE',  ( -3.999999999999996447, -8.999999999999992895, 18.00000000000000000 ) ) ;
#5441 = CARTESIAN_POINT ( 'NONE',  ( 2.672651547586948120E-15, 29.07812499938548001, 13.33755215474602984 ) ) ;
#5442 = MECHANICAL_DESIGN_GEOMETRIC_PRESENTATION_REPRESENTATION (  '', ( #23407 ), #459 ) ;
#5443 = CYLINDRICAL_SURFACE ( 'NONE', #379, 31.10000000000000142 ) ;
#5444 = CARTESIAN_POINT ( 'NONE',  ( 17.29753586877772520, 19.95373324673703408, 12.25316411605951927 ) ) ;
#5445 = LINE ( 'NONE', #13676, #1705 ) ;
#5446 = ORIENTED_EDGE ( 'NONE', *, *, #10740, .T. ) ;
#5447 = DIRECTION ( 'NONE',  ( -0.000000000000000000, -0.000000000000000000, 1.000000000000000000 ) ) ;
#5448 = CARTESIAN_POINT ( 'NONE',  ( -1.878215178124998497, 25.55312499938548854, 12.25316411605951927 ) ) ;
#5449 = CARTESIAN_POINT ( 'NONE',  ( 1.878215178124995832, -28.44062499938548427, 5.746835883940462963 ) ) ;
#5451 = ORIENTED_EDGE ( 'NONE', *, *, #8498, .F. ) ;
#5450 = CARTESIAN_POINT ( 'NONE',  ( 2.000000000000000888, 29.42500000000000071, 12.46410161513774817 ) ) ;
#5452 = CARTESIAN_POINT ( 'NONE',  ( 1.878215178125004048, 26.67812499938548498, 5.746835883940462963 ) ) ;
#5453 = AXIS2_PLACEMENT_3D ( 'NONE', #7275, #15251, #17705 ) ;
#5454 = CARTESIAN_POINT ( 'NONE',  ( 24.67207871933482011, 8.377607117416825844, 20.00001200000000168 ) ) ;
#5455 = CARTESIAN_POINT ( 'NONE',  ( -1.878215178125004048, -28.81562499938548427, 5.746835883940462963 ) ) ;
#5456 = ORIENTED_EDGE ( 'NONE', *, *, #12069, .F. ) ;
#5457 = ORIENTED_EDGE ( 'NONE', *, *, #3624, .T. ) ;
#5458 = SURFACE_STYLE_USAGE ( .BOTH. , #13309 ) ;
#5459 = CARTESIAN_POINT ( 'NONE',  ( 0.000000000000000000, 25.92812499938548854, 13.33755215474602984 ) ) ;
#5460 = VECTOR ( 'NONE', #7378, 1000.000000000000000 ) ;
#5461 = CARTESIAN_POINT ( 'NONE',  ( -1.878215178124995832, -5.746835883940462963, 0.7406249993854828739 ) ) ;
#5462 = AXIS2_PLACEMENT_3D ( 'NONE', #18661, #4675, #8596 ) ;
#5463 = CARTESIAN_POINT ( 'NONE',  ( 1.878215178125000939, -12.25316411605952283, 3.328124999385485783 ) ) ;
#5464 = EDGE_CURVE ( 'NONE', #2244, #1666, #23131, .T. ) ;
#5465 = DIRECTION ( 'NONE',  ( -1.000000000000000000, -0.000000000000000000, -0.000000000000000000 ) ) ;
#5466 = AXIS2_PLACEMENT_3D ( 'NONE', #25473, #21295, #7307 ) ;
#5467 = DIRECTION ( 'NONE',  ( -0.7071067811865487940, -0.7071067811865463515, 0.000000000000000000 ) ) ;
#5468 = DIRECTION ( 'NONE',  ( 0.000000000000000000, 0.000000000000000000, 1.000000000000000000 ) ) ;
#5469 = CARTESIAN_POINT ( 'NONE',  ( -3.999999999999995559, 26.53750000000000142, 6.690598923241487306 ) ) ;
#5470 = DIRECTION ( 'NONE',  ( -0.000000000000000000, 0.000000000000000000, 1.000000000000000000 ) ) ;
#5471 = CARTESIAN_POINT ( 'NONE',  ( -30.04913349766215802, 5.827558883616378083, 1.000000000000000000 ) ) ;
#5472 = CARTESIAN_POINT ( 'NONE',  ( 17.28434138175965273, 20.11276850650576975, 5.535898384862237620 ) ) ;
#5473 = ORIENTED_EDGE ( 'NONE', *, *, #19553, .T. ) ;
#5474 = DIRECTION ( 'NONE',  ( -0.000000000000000000, -0.000000000000000000, -1.000000000000000000 ) ) ;
#5475 = DIRECTION ( 'NONE',  ( 0.000000000000000000, 0.000000000000000000, -1.000000000000000000 ) ) ;
#5476 = CARTESIAN_POINT ( 'NONE',  ( 3.756430356250004099, 28.44062499938548783, 6.831223922626973533 ) ) ;
#5478 = EDGE_CURVE ( 'NONE', #23155, #20629, #13939, .T. ) ;
#5477 = CARTESIAN_POINT ( 'NONE',  ( 21.11597625318330884, 15.45912200369085632, 11.30940107675849760 ) ) ;
#5479 = AXIS2_PLACEMENT_3D ( 'NONE', #1632, #5682, #13933 ) ;
#5480 = CARTESIAN_POINT ( 'NONE',  ( 1.071796769724495668, 27.15759618943233633, 12.99999999999999112 ) ) ;
#5481 = CARTESIAN_POINT ( 'NONE',  ( 1.773386257881301553, -29.94852044693267246, 12.59496732558994125 ) ) ;
#5482 = EDGE_LOOP ( 'NONE', ( #8971, #21408, #11403, #25710 ) ) ;
#5483 = DIRECTION ( 'NONE',  ( 0.000000000000000000, 0.000000000000000000, 1.000000000000000000 ) ) ;
#5484 = ORIENTED_EDGE ( 'NONE', *, *, #8353, .T. ) ;
#5485 = ADVANCED_FACE ( 'NONE', ( #7973 ), #6010, .F. ) ;
#5486 = AXIS2_PLACEMENT_3D ( 'NONE', #4417, #8344, #16332 ) ;
#5487 = ORIENTED_EDGE ( 'NONE', *, *, #3339, .F. ) ;
#5488 = VERTEX_POINT ( 'NONE', #18432 ) ;
#5489 = ORIENTED_EDGE ( 'NONE', *, *, #7117, .T. ) ;
#5490 = ADVANCED_FACE ( 'NONE', ( #16987 ), #20647, .F. ) ;
#5491 = ORIENTED_EDGE ( 'NONE', *, *, #14403, .T. ) ;
#5492 = DIRECTION ( 'NONE',  ( 0.000000000000000000, 0.000000000000000000, 1.000000000000000000 ) ) ;
#5494 = DIRECTION ( 'NONE',  ( 1.000000000000000000, 0.000000000000000000, -0.000000000000000000 ) ) ;
#5493 = AXIS2_PLACEMENT_3D ( 'NONE', #21398, #25057, #16960 ) ;
#5495 = DIRECTION ( 'NONE',  ( 0.000000000000000000, 0.000000000000000000, 1.000000000000000000 ) ) ;
#5496 = EDGE_CURVE ( 'NONE', #14487, #19630, #18118, .T. ) ;
#5497 = CIRCLE ( 'NONE', #8006, 0.5000000000000001110 ) ;
#5498 = CARTESIAN_POINT ( 'NONE',  ( -1.878215178124998497, -12.25316411605951927, 3.590624999385481075 ) ) ;
#5499 = CARTESIAN_POINT ( 'NONE',  ( -1.999999999999998224, -12.46410161513774639, 1.143749998770968279 ) ) ;
#5500 = CARTESIAN_POINT ( 'NONE',  ( 30.45149776762725224, -6.317933499823547017, -2.750000000000000000 ) ) ;
#5501 = CIRCLE ( 'NONE', #14293, 0.5000000000000002220 ) ;
#5502 = CARTESIAN_POINT ( 'NONE',  ( 3.756430356250002323, 27.46562499938548640, 11.16877607737301226 ) ) ;
#5503 = AXIS2_PLACEMENT_3D ( 'NONE', #4864, #11128, #19106 ) ;
#5504 = CARTESIAN_POINT ( 'NONE',  ( -4.000000000000003553, -26.78124999877097068, 6.690598923241489970 ) ) ;
#5505 = CARTESIAN_POINT ( 'NONE',  ( -22.32573188046898238, 21.65113613650357749, 1.000000000000000000 ) ) ;
#5506 = CARTESIAN_POINT ( 'NONE',  ( 4.000000000000003553, -8.999999999999992895, 2.700000000000001066 ) ) ;
#5507 = DIRECTION ( 'NONE',  ( 0.000000000000000000, 0.000000000000000000, 1.000000000000000000 ) ) ;
#5508 = CARTESIAN_POINT ( 'NONE',  ( -5.335677986744467027, 30.63887302793251877, 1.000000000000000000 ) ) ;
#5509 = CARTESIAN_POINT ( 'NONE',  ( -1.626862140677534194E-14, -28.43124999877096570, 12.99999999999999289 ) ) ;
#5510 = CARTESIAN_POINT ( 'NONE',  ( 3.999999999999997335, -27.00624999877096499, 11.30940107675849404 ) ) ;
#5511 = AXIS2_PLACEMENT_3D ( 'NONE', #22692, #6338, #2797 ) ;
#5512 = CARTESIAN_POINT ( 'NONE',  ( 4.000000000000003553, 29.89374999877096784, 8.999999999999992895 ) ) ;
#5513 = DIRECTION ( 'NONE',  ( 0.000000000000000000, 0.000000000000000000, -1.000000000000000000 ) ) ;
#5514 = DIRECTION ( 'NONE',  ( -0.7071067811865487940, -0.7071067811865463515, 0.000000000000000000 ) ) ;
#5515 = CARTESIAN_POINT ( 'NONE',  ( 25.45105997952925136, 17.87326343783933780, -2.750000000000000000 ) ) ;
#5516 = ORIENTED_EDGE ( 'NONE', *, *, #14033, .T. ) ;
#5517 = CARTESIAN_POINT ( 'NONE',  ( 1.952785157361650370, 31.03863125411924528, -6.500000000000000000 ) ) ;
#5518 = ORIENTED_EDGE ( 'NONE', *, *, #22622, .F. ) ;
#5519 = CIRCLE ( 'NONE', #15987, 0.5000000000000002220 ) ;
#5520 = ORIENTED_EDGE ( 'NONE', *, *, #23366, .T. ) ;
#5521 = DIRECTION ( 'NONE',  ( 1.000000000000000000, 0.000000000000000000, 0.000000000000000000 ) ) ;
#5522 =( BOUNDED_CURVE ( )  B_SPLINE_CURVE ( 2, ( #2149, #14438, #4616, #10351, #449, #8420, #14173, #12598, #16408 ),
 .UNSPECIFIED., .F., .F. ) 
 B_SPLINE_CURVE_WITH_KNOTS ( ( 3, 2, 2, 2, 3 ),
 ( 0.2250000000000000056, 0.2333333333333333370, 0.2500000000000000000, 0.2666666666666666630, 0.2750000000000000222 ),
 .UNSPECIFIED. ) 
 CURVE ( )  GEOMETRIC_REPRESENTATION_ITEM ( )  RATIONAL_B_SPLINE_CURVE ( ( 0.9330127018922194093, 0.9330127018922194093, 1.000000000000000000, 0.8660254037844387076, 1.000000000000000000, 0.8660254037844387076, 1.000000000000000000, 0.9330127018922191873, 0.9330127018922194093 ) ) 
 REPRESENTATION_ITEM ( '' )  );
#5523 = ORIENTED_EDGE ( 'NONE', *, *, #10900, .T. ) ;
#5524 = CARTESIAN_POINT ( 'NONE',  ( -3.756430356250004099, -27.99062499938548498, 6.831223922626973533 ) ) ;
#5525 = EDGE_CURVE ( 'NONE', #24045, #1951, #12693, .T. ) ;
#5526 = ORIENTED_EDGE ( 'NONE', *, *, #16679, .F. ) ;
#5527 = CARTESIAN_POINT ( 'NONE',  ( -1.071796769724488563, 28.91740381056766651, 12.99999999999999289 ) ) ;
#5528 = EDGE_CURVE ( 'NONE', #9327, #17764, #2051, .T. ) ;
#5529 = CIRCLE ( 'NONE', #7191, 4.000000000000000000 ) ;
#5530 = VERTEX_POINT ( 'NONE', #20370 ) ;
#5531 = VECTOR ( 'NONE', #11693, 1000.000000000000000 ) ;
#5532 = CARTESIAN_POINT ( 'NONE',  ( -1.999999999999998224, 28.44999999999999929, 12.46410161513774639 ) ) ;
#5533 = EDGE_CURVE ( 'NONE', #8698, #2116, #2610, .T. ) ;
#5534 = CARTESIAN_POINT ( 'NONE',  ( 1.071796769724491671, 29.40759618943233633, 12.99999999999999467 ) ) ;
#5535 = CIRCLE ( 'NONE', #23070, 31.10000000000000142 ) ;
#5536 = CARTESIAN_POINT ( 'NONE',  ( -1.859271017917182139E-15, -29.33124999877096428, 12.99999999999999289 ) ) ;
#5537 = LINE ( 'NONE', #13521, #9575 ) ;
#5538 = CARTESIAN_POINT ( 'NONE',  ( 17.87862548900172044, 23.19102024492039504, 6.831223922626973533 ) ) ;
#5539 = DIRECTION ( 'NONE',  ( -0.7071067811865487940, -0.7071067811865463515, 0.000000000000000000 ) ) ;
#5540 = AXIS2_PLACEMENT_3D ( 'NONE', #6642, #15396, #21282 ) ;
#5541 = EDGE_CURVE ( 'NONE', #10843, #11941, #22552, .T. ) ;
#5542 = CARTESIAN_POINT ( 'NONE',  ( 3.756430356250003655, 29.64062499938548356, 8.999999999999992895 ) ) ;
#5543 = CARTESIAN_POINT ( 'NONE',  ( 20.32269083260512588, 20.32269083260505482, 13.33755215474603162 ) ) ;
#5544 = DIRECTION ( 'NONE',  ( 1.000000000000000000, 0.000000000000000000, 0.000000000000000000 ) ) ;
#5545 = ORIENTED_EDGE ( 'NONE', *, *, #11555, .T. ) ;
#5546 = ORIENTED_EDGE ( 'NONE', *, *, #2336, .F. ) ;
#5547 = CARTESIAN_POINT ( 'NONE',  ( 2.000000000000000000, 28.46874999877097423, 12.46410161513774817 ) ) ;
#5548 = ORIENTED_EDGE ( 'NONE', *, *, #2666, .F. ) ;
#5549 = DIRECTION ( 'NONE',  ( 0.000000000000000000, -0.000000000000000000, 1.000000000000000000 ) ) ;
#5550 = AXIS2_PLACEMENT_3D ( 'NONE', #3299, #1873, #25783 ) ;
#5551 = EDGE_CURVE ( 'NONE', #24860, #13686, #19362, .T. ) ;
#5552 = CARTESIAN_POINT ( 'NONE',  ( 3.735045420075836212E-15, 28.96562499938548640, 4.662447845253954171 ) ) ;
#5553 = CARTESIAN_POINT ( 'NONE',  ( -1.071796769724490117, 27.32634618820330630, 4.999999999999992895 ) ) ;
#5554 = ORIENTED_EDGE ( 'NONE', *, *, #7444, .F. ) ;
#5555 = ORIENTED_EDGE ( 'NONE', *, *, #18400, .T. ) ;
#5556 = EDGE_CURVE ( 'NONE', #21696, #1445, #16481, .T. ) ;
#5557 = AXIS2_PLACEMENT_3D ( 'NONE', #12605, #2670, #24767 ) ;
#5558 = FACE_OUTER_BOUND ( 'NONE', #6328, .T. ) ;
#5559 = ORIENTED_EDGE ( 'NONE', *, *, #12177, .T. ) ;
#5560 = CARTESIAN_POINT ( 'NONE',  ( 0.1550712154453031122, 38.97879272568130204, 14.51938357696415416 ) ) ;
#5561 = CARTESIAN_POINT ( 'NONE',  ( 1.878215178125004048, 25.21562499938548285, 5.746835883940462963 ) ) ;
#5562 = CARTESIAN_POINT ( 'NONE',  ( -3.756430356249997882, 28.10312499938548569, 11.16877607737301048 ) ) ;
#5563 = FACE_OUTER_BOUND ( 'NONE', #10420, .T. ) ;
#5564 = CARTESIAN_POINT ( 'NONE',  ( -1.999999999999998224, 27.10000000000000497, 12.46410161513774639 ) ) ;
#5565 =( BOUNDED_CURVE ( )  B_SPLINE_CURVE ( 2, ( #24882, #11132, #6960, #14939, #3044, #19110, #18994, #1077, #7224 ),
 .UNSPECIFIED., .F., .F. ) 
 B_SPLINE_CURVE_WITH_KNOTS ( ( 3, 2, 2, 2, 3 ),
 ( 0.07500000000000001110, 0.08333333333333332871, 0.1000000000000000056, 0.1166666666666666685, 0.1250000000000000000 ),
 .UNSPECIFIED. ) 
 CURVE ( )  GEOMETRIC_REPRESENTATION_ITEM ( )  RATIONAL_B_SPLINE_CURVE ( ( 0.9330127018922192983, 0.9330127018922194093, 1.000000000000000000, 0.8660254037844387076, 1.000000000000000000, 0.8660254037844387076, 1.000000000000000000, 0.9330127018922194093, 0.9330127018922194093 ) ) 
 REPRESENTATION_ITEM ( '' )  );
#5566 = EDGE_CURVE ( 'NONE', #20798, #22527, #8189, .T. ) ;
#5567 = AXIS2_PLACEMENT_3D ( 'NONE', #458, #24384, #14448 ) ;
#5568 = CARTESIAN_POINT ( 'NONE',  ( -3.756430356249996994, 27.61562499938548143, 8.999999999999992895 ) ) ;
#5569 = DIRECTION ( 'NONE',  ( -0.9297764858882481276, 0.3681245526846864125, 0.000000000000000000 ) ) ;
#5570 = DIRECTION ( 'NONE',  ( 0.000000000000000000, -0.000000000000000000, 1.000000000000000000 ) ) ;
#5571 = COLOUR_RGB ( '',0.8941176470588234615, 0.8941176470588234615, 0.8941176470588234615 ) ;
#5572 = CARTESIAN_POINT ( 'NONE',  ( 3.756430356250002323, 27.80312499938548143, 11.16877607737301403 ) ) ;
#5573 = CARTESIAN_POINT ( 'NONE',  ( 0.000000000000000000, 0.000000000000000000, 19.00000000000000000 ) ) ;
#5574 = CARTESIAN_POINT ( 'NONE',  ( 16.25461713252580509, 21.91147138201811373, 6.690598923241487306 ) ) ;
#5575 = CARTESIAN_POINT ( 'NONE',  ( 19.36809667800328683, 19.36809667800321932, 13.33755215474602984 ) ) ;
#5576 = LINE ( 'NONE', #9622, #24714 ) ;
#5577 = CARTESIAN_POINT ( 'NONE',  ( 1.071796769724494558, 28.24240381056766580, 4.999999999999992895 ) ) ;
#5578 = DIRECTION ( 'NONE',  ( 1.000000000000000000, 0.000000000000000000, 0.000000000000000000 ) ) ;
#5579 = CARTESIAN_POINT ( 'NONE',  ( 23.27056975780394765, 17.95817500188513094, 11.16877607737301403 ) ) ;
#5580 = DIRECTION ( 'NONE',  ( 0.000000000000000000, 0.000000000000000000, 1.000000000000000000 ) ) ;
#5581 = VERTEX_POINT ( 'NONE', #14892 ) ;
#5582 = CARTESIAN_POINT ( 'NONE',  ( 4.000000000000003553, 25.84374999877096712, 8.999999999999992895 ) ) ;
#5583 = CARTESIAN_POINT ( 'NONE',  ( -2.000000000000000888, -25.82499999999999929, 12.46410161513774817 ) ) ;
#5585 = VERTEX_POINT ( 'NONE', #22475 ) ;
#5584 = CARTESIAN_POINT ( 'NONE',  ( 1.859271017917182139E-15, 29.38749999999999929, 12.99999999999999289 ) ) ;
#5586 = DIRECTION ( 'NONE',  ( 0.000000000000000000, 0.000000000000000000, 1.000000000000000000 ) ) ;
#5587 = LINE ( 'NONE', #19558, #15941 ) ;
#5588 =( GEOMETRIC_REPRESENTATION_CONTEXT ( 3 ) GLOBAL_UNCERTAINTY_ASSIGNED_CONTEXT ( ( #16739 ) ) GLOBAL_UNIT_ASSIGNED_CONTEXT ( ( #16351, #10186, #6015 ) ) REPRESENTATION_CONTEXT ( 'NONE', 'WORKASPACE' ) );
#5589 = CARTESIAN_POINT ( 'NONE',  ( -26.00000000000000000, 1.701696020694461131, 20.00001199999999812 ) ) ;
#5590 = FACE_OUTER_BOUND ( 'NONE', #19770, .T. ) ;
#5591 = ORIENTED_EDGE ( 'NONE', *, *, #6167, .T. ) ;
#5592 = ORIENTED_EDGE ( 'NONE', *, *, #21469, .F. ) ;
#5593 = PRESENTATION_STYLE_ASSIGNMENT (( #5458 ) ) ;
#5594 = CARTESIAN_POINT ( 'NONE',  ( -1.878215178124998275, 25.44062499938549138, 12.25316411605951927 ) ) ;
#5595 = AXIS2_PLACEMENT_3D ( 'NONE', #23338, #25310, #23101 ) ;
#5596 = EDGE_CURVE ( 'NONE', #18495, #14524, #8497, .T. ) ;
#5597 = CARTESIAN_POINT ( 'NONE',  ( 3.756430356250003211, -6.831223922626973533, 0.1781249993854828739 ) ) ;
#5598 = CARTESIAN_POINT ( 'NONE',  ( 1.878215178125000939, -12.25316411605952283, 4.228124999385483918 ) ) ;
#5599 = FILL_AREA_STYLE ('',( #19571 ) ) ;
#5600 = FACE_OUTER_BOUND ( 'NONE', #10710, .T. ) ;
#5601 = CARTESIAN_POINT ( 'NONE',  ( 24.00000000000000355, 0.000000000000000000, 17.00000000000000000 ) ) ;
#5602 = CYLINDRICAL_SURFACE ( 'NONE', #16774, 0.5000000000000004441 ) ;
#5603 = CARTESIAN_POINT ( 'NONE',  ( -0.5788183228083377818, -29.99578766836522092, 12.96878440844335678 ) ) ;
#5604 = DIRECTION ( 'NONE',  ( 0.000000000000000000, 1.000000000000000000, 0.000000000000000000 ) ) ;
#5605 = CARTESIAN_POINT ( 'NONE',  ( 17.39040739893763643, 20.21883452368375700, 12.46410161513774639 ) ) ;
#5606 = VERTEX_POINT ( 'NONE', #12536 ) ;
#5607 = CARTESIAN_POINT ( 'NONE',  ( 5.840899737312971851, 38.49999999999999289, 7.627451181685208859 ) ) ;
#5608 = DIRECTION ( 'NONE',  ( -0.1873813145857119722, 0.9822872507286911636, 0.000000000000000000 ) ) ;
#5609 = CARTESIAN_POINT ( 'NONE',  ( 3.735045420075836212E-15, 28.06562499938548427, 4.662447845253954171 ) ) ;
#5610 = CARTESIAN_POINT ( 'NONE',  ( -1.071796769724487230, 25.97634618820330132, 4.999999999999992006 ) ) ;
#5611 = CARTESIAN_POINT ( 'NONE',  ( 3.884165915710650729, 38.55544002051693298, 13.50011709117523218 ) ) ;
#5612 = ORIENTED_EDGE ( 'NONE', *, *, #25472, .F. ) ;
#5613 = CARTESIAN_POINT ( 'NONE',  ( 1.999999999999995781, -26.89374999877097139, 5.535898384862237620 ) ) ;
#5614 = LINE ( 'NONE', #1694, #7938 ) ;
#5616 = VERTEX_POINT ( 'NONE', #16869 ) ;
#5615 = CARTESIAN_POINT ( 'NONE',  ( -25.99519186311192342, -0.5000000000000000000, 19.50000000000000000 ) ) ;
#5617 = EDGE_LOOP ( 'NONE', ( #10086, #20543, #3451, #1447 ) ) ;
#5618 = ORIENTED_EDGE ( 'NONE', *, *, #21163, .T. ) ;
#5619 = ORIENTED_EDGE ( 'NONE', *, *, #13131, .T. ) ;
#5620 = EDGE_LOOP ( 'NONE', ( #18203, #5939, #5326, #19028 ) ) ;
#5621 = CARTESIAN_POINT ( 'NONE',  ( 1.500000000000001776, -10.49999999999999289, 30.00000000000000355 ) ) ;
#5622 = CARTESIAN_POINT ( 'NONE',  ( 17.91631806831418317, 17.91631806831411922, 12.99999999999999289 ) ) ;
#5623 = ADVANCED_FACE ( 'NONE', ( #24834 ), #18948, .F. ) ;
#5624 = AXIS2_PLACEMENT_3D ( 'NONE', #7720, #19748, #15823 ) ;
#5625 = CARTESIAN_POINT ( 'NONE',  ( 1.999999999999998224, -29.35000000000000142, 12.46410161513774639 ) ) ;
#5626 = FACE_OUTER_BOUND ( 'NONE', #3399, .T. ) ;
#5627 = EDGE_CURVE ( 'NONE', #19467, #23600, #1033, .T. ) ;
#5628 = CARTESIAN_POINT ( 'NONE',  ( 1.878215178125004048, -5.746835883940462963, 3.815624999385484273 ) ) ;
#5629 = CARTESIAN_POINT ( 'NONE',  ( 2.620986760973688460E-15, -13.61880215351699874, 2.981249998770966414 ) ) ;
#5630 = EDGE_CURVE ( 'NONE', #1683, #13534, #1540, .T. ) ;
#5631 = CARTESIAN_POINT ( 'NONE',  ( -3.756430356249995661, 28.59062499938548640, 6.831223922626973533 ) ) ;
#5632 = DIRECTION ( 'NONE',  ( 0.000000000000000000, 0.000000000000000000, 1.000000000000000000 ) ) ;
#5633 = CARTESIAN_POINT ( 'NONE',  ( -23.46296185032722548, -19.82388608118403539, 1.000000000000000000 ) ) ;
#5634 = CARTESIAN_POINT ( 'NONE',  ( 2.000000000000000888, -12.46410161513774817, 1.725000000000000755 ) ) ;
#5635 = CARTESIAN_POINT ( 'NONE',  ( -4.000000000000003553, -25.88124999877096855, 6.690598923241489970 ) ) ;
#5637 = EDGE_CURVE ( 'NONE', #3578, #13216, #3233, .T. ) ;
#5636 = DIRECTION ( 'NONE',  ( 0.000000000000000000, 1.000000000000000000, 0.000000000000000000 ) ) ;
#5638 = CYLINDRICAL_SURFACE ( 'NONE', #23480, 4.000000000000000000 ) ;
#5639 = CARTESIAN_POINT ( 'NONE',  ( 3.999999999999996447, -26.96874999877096712, 8.999999999999992895 ) ) ;
#5640 = CARTESIAN_POINT ( 'NONE',  ( 1.878215178125000939, 27.87812499938548427, 12.25316411605952283 ) ) ;
#5641 = DIRECTION ( 'NONE',  ( 1.000000000000000000, 0.000000000000000000, 0.000000000000000000 ) ) ;
#5642 = CARTESIAN_POINT ( 'NONE',  ( 4.000000000000001776, -11.30940107675849760, 4.856249998770968190 ) ) ;
#5643 = DIRECTION ( 'NONE',  ( 1.000000000000000000, 0.000000000000000000, 0.000000000000000000 ) ) ;
#5644 = ORIENTED_EDGE ( 'NONE', *, *, #17773, .T. ) ;
#5645 = FACE_OUTER_BOUND ( 'NONE', #22995, .T. ) ;
#5646 = EDGE_LOOP ( 'NONE', ( #5869, #131, #23428, #24013 ) ) ;
#5647 = EDGE_LOOP ( 'NONE', ( #11883, #20433, #19088, #5546, #2141, #19856 ) ) ;
#5648 = DIRECTION ( 'NONE',  ( 0.000000000000000000, 0.000000000000000000, 1.000000000000000000 ) ) ;
#5649 = EDGE_LOOP ( 'NONE', ( #18202, #7829, #9947, #14142 ) ) ;
#5650 = CARTESIAN_POINT ( 'NONE',  ( 1.878215178124995832, -27.20312499938548711, 5.746835883940462963 ) ) ;
#5651 = VERTEX_POINT ( 'NONE', #21423 ) ;
#5652 = CARTESIAN_POINT ( 'NONE',  ( -0.7500000000000001110, 9.184850993605150903E-17, 15.00000000000000178 ) ) ;
#5653 = ORIENTED_EDGE ( 'NONE', *, *, #7234, .T. ) ;
#5654 = CARTESIAN_POINT ( 'NONE',  ( 2.000000000000000888, 27.17500000000000071, 12.46410161513774817 ) ) ;
#5655 = DIRECTION ( 'NONE',  ( 0.9822872507286884991, -0.1873813145857256834, 0.000000000000000000 ) ) ;
#5656 = EDGE_CURVE ( 'NONE', #2042, #13143, #11430, .T. ) ;
#5657 = VECTOR ( 'NONE', #24572, 1000.000000000000000 ) ;
#5658 = FACE_OUTER_BOUND ( 'NONE', #23123, .T. ) ;
#5659 = FACE_OUTER_BOUND ( 'NONE', #15278, .T. ) ;
#5660 = CARTESIAN_POINT ( 'NONE',  ( 19.15823811790222919, 16.50204073994278531, 5.746835883940462963 ) ) ;
#5661 = PLANE ( 'NONE',  #18398 ) ;
#5662 = EDGE_CURVE ( 'NONE', #13093, #6968, #25229, .T. ) ;
#5663 = CARTESIAN_POINT ( 'NONE',  ( -3.999999999999996003, 27.43750000000000000, 6.690598923241487306 ) ) ;
#5664 = EDGE_CURVE ( 'NONE', #14041, #13717, #169, .T. ) ;
#5665 = FACE_OUTER_BOUND ( 'NONE', #18463, .T. ) ;
#5666 = CARTESIAN_POINT ( 'NONE',  ( 23.37663577498192780, 18.06424101906310753, 8.999999999999992895 ) ) ;
#5667 = CARTESIAN_POINT ( 'NONE',  ( -22.67092431280563503, 21.28941499438250062, -6.500000000000000000 ) ) ;
#5668 = VERTEX_POINT ( 'NONE', #4794 ) ;
#5669 = ORIENTED_EDGE ( 'NONE', *, *, #10339, .F. ) ;
#5670 = CARTESIAN_POINT ( 'NONE',  ( 2.000000000000000000, 29.81874999877097210, 12.46410161513774817 ) ) ;
#5671 = ORIENTED_EDGE ( 'NONE', *, *, #1035, .T. ) ;
#5672 = FACE_OUTER_BOUND ( 'NONE', #1917, .T. ) ;
#5673 = CARTESIAN_POINT ( 'NONE',  ( -1.878215178124995832, 28.10312499938548569, 5.746835883940462963 ) ) ;
#5674 = CARTESIAN_POINT ( 'NONE',  ( 4.000000000000003553, 28.09374999877097068, 8.999999999999992895 ) ) ;
#5675 = ORIENTED_EDGE ( 'NONE', *, *, #3328, .T. ) ;
#5676 = ORIENTED_EDGE ( 'NONE', *, *, #8645, .T. ) ;
#5677 = CARTESIAN_POINT ( 'NONE',  ( 7.901901826148023498E-15, 27.53124999877097068, 12.99999999999999112 ) ) ;
#5678 = ORIENTED_EDGE ( 'NONE', *, *, #18962, .F. ) ;
#5679 = FACE_OUTER_BOUND ( 'NONE', #25492, .T. ) ;
#5680 = CARTESIAN_POINT ( 'NONE',  ( 26.52310962334739486, -16.23990935651726275, -6.500000000000000000 ) ) ;
#5681 = CARTESIAN_POINT ( 'NONE',  ( -3.756430356249994773, 28.96562499938548640, 8.999999999999992895 ) ) ;
#5682 = DIRECTION ( 'NONE',  ( 0.000000000000000000, 0.000000000000000000, 1.000000000000000000 ) ) ;
#5683 = CARTESIAN_POINT ( 'NONE',  ( -3.999999999999994671, 27.88750000000000639, 6.690598923241487306 ) ) ;
#5684 = EDGE_CURVE ( 'NONE', #23080, #13703, #5170, .T. ) ;
#5685 = DIRECTION ( 'NONE',  ( 0.000000000000000000, 0.000000000000000000, 1.000000000000000000 ) ) ;
#5686 = DIRECTION ( 'NONE',  ( 0.000000000000000000, 0.000000000000000000, 1.000000000000000000 ) ) ;
#5687 = EDGE_CURVE ( 'NONE', #7768, #17145, #734, .T. ) ;
#5688 = CARTESIAN_POINT ( 'NONE',  ( -4.000000000000039968, -11.30940107675846740, 1.106249998770968634 ) ) ;
#5689 = CARTESIAN_POINT ( 'NONE',  ( 2.000000000000000888, 28.97500000000000142, 12.46410161513774817 ) ) ;
#5690 = CARTESIAN_POINT ( 'NONE',  ( 3.110308778861319734, 34.50000000000000000, 3.869115154270335477 ) ) ;
#5691 = CARTESIAN_POINT ( 'NONE',  ( 22.09708691207964293, 16.44023266258718863, 8.999999999999992895 ) ) ;
#5692 = CARTESIAN_POINT ( 'NONE',  ( 19.28627369086489551, 21.94247106882419729, 12.25316411605951927 ) ) ;
#5693 = CARTESIAN_POINT ( 'NONE',  ( -28.14012133169306296, 13.24173596767408867, -6.500000000000000000 ) ) ;
#5694 = CARTESIAN_POINT ( 'NONE',  ( 2.000000000000003997, 29.51874999877096784, 5.535898384862238508 ) ) ;
#5695 = CARTESIAN_POINT ( 'NONE',  ( 2.000000000000000000, 27.11874999877097281, 12.46410161513774817 ) ) ;
#5696 = CARTESIAN_POINT ( 'NONE',  ( 20.87953742278953229, 20.87953742278946123, 13.33755215474603162 ) ) ;
#5697 = DIRECTION ( 'NONE',  ( 0.000000000000000000, 0.000000000000000000, 1.000000000000000000 ) ) ;
#5698 = EDGE_LOOP ( 'NONE', ( #23371, #24133, #23127, #7405 ) ) ;
#5699 = CARTESIAN_POINT ( 'NONE',  ( 2.000000000000003997, 25.91874999877096997, 5.535898384862238508 ) ) ;
#5700 = CARTESIAN_POINT ( 'NONE',  ( 3.999999999999996447, -26.12500000000000355, 8.999999999999992895 ) ) ;
#5702 = ORIENTED_EDGE ( 'NONE', *, *, #15200, .T. ) ;
#5701 = CARTESIAN_POINT ( 'NONE',  ( 3.756430356250003211, 25.70312499938548356, 8.999999999999992895 ) ) ;
#5703 = CARTESIAN_POINT ( 'NONE',  ( 1.878215178125004048, 27.57812499938548711, 5.746835883940462963 ) ) ;
#5704 = DIRECTION ( 'NONE',  ( 0.000000000000000000, 1.000000000000000000, 0.000000000000000000 ) ) ;
#5705 = CARTESIAN_POINT ( 'NONE',  ( 25.83240171513483929, 3.403349963601484340, 20.00001200000000168 ) ) ;
#5706 = DIRECTION ( 'NONE',  ( -1.000000000000000000, 0.000000000000000000, 0.000000000000000000 ) ) ;
#5707 = ORIENTED_EDGE ( 'NONE', *, *, #6994, .F. ) ;
#5708 = ORIENTED_EDGE ( 'NONE', *, *, #14297, .T. ) ;
#5709 = DIRECTION ( 'NONE',  ( 0.000000000000000000, -1.000000000000000000, 0.000000000000000000 ) ) ;
#5710 = CARTESIAN_POINT ( 'NONE',  ( 0.000000000000000000, 29.64062499938549422, 13.33755215474602984 ) ) ;
#5711 =( BOUNDED_CURVE ( )  B_SPLINE_CURVE ( 2, ( #24376, #4229, #24493, #4091, #22534, #16141, #16532 ),
 .UNSPECIFIED., .F., .T. ) 
 B_SPLINE_CURVE_WITH_KNOTS ( ( 3, 2, 2, 3 ),
 ( 0.3999999999999999667, 0.4166666666666665741, 0.4333333333333332371, 0.4499999999999998446 ),
 .UNSPECIFIED. ) 
 CURVE ( )  GEOMETRIC_REPRESENTATION_ITEM ( )  RATIONAL_B_SPLINE_CURVE ( ( 1.000000000000000444, 0.8660254037844382635, 1.000000000000000000, 0.8660254037844387076, 1.000000000000000000, 0.8660254037844400399, 0.9999999999999986677 ) ) 
 REPRESENTATION_ITEM ( '' )  );
#5712 = CARTESIAN_POINT ( 'NONE',  ( 2.672651547586948120E-15, -13.33755215474603162, 2.728124999385481253 ) ) ;
#5713 = AXIS2_PLACEMENT_3D ( 'NONE', #22301, #20449, #12355 ) ;
#5714 = CARTESIAN_POINT ( 'NONE',  ( 1.487416814333745711E-14, 28.43124999877096926, 12.99999999999999289 ) ) ;
#5715 = ADVANCED_FACE ( 'NONE', ( #10781 ), #2818, .F. ) ;
#5716 = CARTESIAN_POINT ( 'NONE',  ( -3.834746474454188013E-15, -27.75624999877096855, 4.999999999999992006 ) ) ;
#5717 = CARTESIAN_POINT ( 'NONE',  ( 22.07057040778514789, 16.41371615829269359, 11.30940107675849760 ) ) ;
#5718 = DIRECTION ( 'NONE',  ( -0.7705132427757840352, 0.6374239897486960738, 0.000000000000000000 ) ) ;
#5719 = CARTESIAN_POINT ( 'NONE',  ( -11.44867358849309547, 28.91604871112477326, 1.000000000000000000 ) ) ;
#5720 = CARTESIAN_POINT ( 'NONE',  ( 4.000000000000003553, -8.999999999999992895, 2.193749998770967213 ) ) ;
#5721 = CARTESIAN_POINT ( 'NONE',  ( 17.70860545047158396, 20.53703257521770453, 12.46410161513774639 ) ) ;
#5722 = ORIENTED_EDGE ( 'NONE', *, *, #3893, .F. ) ;
#5723 = DIRECTION ( 'NONE',  ( -0.9510565162951518658, 0.3090169943749528914, 0.000000000000000000 ) ) ;
#5724 = CARTESIAN_POINT ( 'NONE',  ( 1.878215178124995832, -29.00312499938548427, 5.746835883940462963 ) ) ;
#5725 = CARTESIAN_POINT ( 'NONE',  ( 3.735045420075836212E-15, 28.51562499938549067, 4.662447845253954171 ) ) ;
#5726 = ADVANCED_FACE ( 'NONE', ( #16691 ), #6489, .T. ) ;
#5727 = DIRECTION ( 'NONE',  ( 0.000000000000000000, 0.000000000000000000, -1.000000000000000000 ) ) ;
#5728 = CARTESIAN_POINT ( 'NONE',  ( -3.999999999999996447, 26.08750000000000213, 6.690598923241487306 ) ) ;
#5729 = CARTESIAN_POINT ( 'NONE',  ( 3.469446951953614189E-15, 31.50000000000000000, 8.999999999999992895 ) ) ;
#5730 = VERTEX_POINT ( 'NONE', #22714 ) ;
#5731 = CARTESIAN_POINT ( 'NONE',  ( -1.999999999999998224, -12.46410161513774639, 2.550000000000000266 ) ) ;
#5732 = CARTESIAN_POINT ( 'NONE',  ( -5.239945491911981890, 38.87560126879805722, 6.955677371495904815 ) ) ;
#5734 = ORIENTED_EDGE ( 'NONE', *, *, #23260, .T. ) ;
#5733 = CARTESIAN_POINT ( 'NONE',  ( 4.000000000000007105, 28.58124999877097139, 6.690598923241489970 ) ) ;
#5735 = EDGE_CURVE ( 'NONE', #18705, #18585, #20613, .T. ) ;
#5736 = ORIENTED_EDGE ( 'NONE', *, *, #10271, .F. ) ;
#5737 = VERTEX_POINT ( 'NONE', #10393 ) ;
#5738 = ORIENTED_EDGE ( 'NONE', *, *, #1001, .F. ) ;
#5739 = ORIENTED_EDGE ( 'NONE', *, *, #4430, .F. ) ;
#5740 = CARTESIAN_POINT ( 'NONE',  ( 13.24173596767359662, -28.14012133169329388, 1.000000000000000000 ) ) ;
#5741 = CARTESIAN_POINT ( 'NONE',  ( -3.057059652155495133, 38.61000136877623135, 14.03455380423570809 ) ) ;
#5742 = DIRECTION ( 'NONE',  ( -0.000000000000000000, -1.000000000000000000, -0.000000000000000000 ) ) ;
#5743 = DIRECTION ( 'NONE',  ( 0.000000000000000000, 0.000000000000000000, 1.000000000000000000 ) ) ;
#5744 = CARTESIAN_POINT ( 'NONE',  ( 3.735045420075836212E-15, -4.662447845253954171, 2.053124999385483207 ) ) ;
#5745 = CARTESIAN_POINT ( 'NONE',  ( 4.000000000000001776, -11.30940107675849760, 4.406249998770963572 ) ) ;
#5746 = CARTESIAN_POINT ( 'NONE',  ( -1.878215178124995832, 27.65312499938548640, 5.746835883940462963 ) ) ;
#5747 = LINE ( 'NONE', #21464, #20471 ) ;
#5748 = CARTESIAN_POINT ( 'NONE',  ( -25.16042852506064165, 18.28012134629622309, -6.500000000000000000 ) ) ;
#5749 = CARTESIAN_POINT ( 'NONE',  ( 2.000000000000003997, -5.535898384862238508, 2.325000000000000622 ) ) ;
#5750 = CYLINDRICAL_SURFACE ( 'NONE', #20461, 0.5000000000000004441 ) ;
#5751 = CARTESIAN_POINT ( 'NONE',  ( -1.999999999999998224, -12.46410161513774639, 2.493749998770968812 ) ) ;
#5752 = DIRECTION ( 'NONE',  ( -0.000000000000000000, -0.000000000000000000, 1.000000000000000000 ) ) ;
#5753 = CARTESIAN_POINT ( 'NONE',  ( -2.000000000000003997, -27.26874999877097139, 5.535898384862238508 ) ) ;
#5754 = CARTESIAN_POINT ( 'NONE',  ( 3.756430356250004099, 28.89062499938548356, 6.831223922626973533 ) ) ;
#5755 = FACE_OUTER_BOUND ( 'NONE', #24409, .T. ) ;
#5756 = ADVANCED_FACE ( 'NONE', ( #18392 ), #490, .F. ) ;
#5757 = CARTESIAN_POINT ( 'NONE',  ( -1.999999999999998224, -12.46410161513774639, 1.649999999999998579 ) ) ;
#5758 = CARTESIAN_POINT ( 'NONE',  ( 3.878215178125001827, 25.07031249969274711, 8.999999999999992895 ) ) ;
#5759 = ORIENTED_EDGE ( 'NONE', *, *, #18309, .T. ) ;
#5760 = FACE_OUTER_BOUND ( 'NONE', #20731, .T. ) ;
#5761 = VERTEX_POINT ( 'NONE', #14862 ) ;
#5762 = EDGE_CURVE ( 'NONE', #20598, #16676, #3477, .T. ) ;
#5763 = ORIENTED_EDGE ( 'NONE', *, *, #20254, .F. ) ;
#5764 = DIRECTION ( 'NONE',  ( -0.7071067811865487940, -0.7071067811865463515, 0.000000000000000000 ) ) ;
#5766 = ORIENTED_EDGE ( 'NONE', *, *, #13029, .F. ) ;
#5765 = CIRCLE ( 'NONE', #2424, 31.10000000000000142 ) ;
#5767 = EDGE_CURVE ( 'NONE', #2145, #11790, #2959, .T. ) ;
#5768 = CARTESIAN_POINT ( 'NONE',  ( -1.878215178125004048, -28.47812499938548569, 5.746835883940462963 ) ) ;
#5769 = EDGE_LOOP ( 'NONE', ( #19394, #18871, #8880, #4766 ) ) ;
#5770 = CYLINDRICAL_SURFACE ( 'NONE', #3430, 4.000000000000000000 ) ;
#5771 = ORIENTED_EDGE ( 'NONE', *, *, #17070, .T. ) ;
#5772 = EDGE_CURVE ( 'NONE', #4968, #5905, #2257, .T. ) ;
#5773 = CARTESIAN_POINT ( 'NONE',  ( -3.999999999999996003, 26.53750000000000142, 6.690598923241487306 ) ) ;
#5774 = CARTESIAN_POINT ( 'NONE',  ( 0.7500000000000001110, 20.00000000000000000, 18.19999999999999929 ) ) ;
#5775 = CARTESIAN_POINT ( 'NONE',  ( -29.57785765677917311, 9.610428525061202265, -6.500000000000000000 ) ) ;
#5776 = CYLINDRICAL_SURFACE ( 'NONE', #9165, 0.5000000000000004441 ) ;
#5777 = CARTESIAN_POINT ( 'NONE',  ( 19.37037015225818948, 16.71417277429875625, 12.25316411605952283 ) ) ;
#5778 = FACE_OUTER_BOUND ( 'NONE', #22339, .T. ) ;
#5779 = CIRCLE ( 'NONE', #7034, 31.10000000000000142 ) ;
#5780 = DIRECTION ( 'NONE',  ( 1.000000000000000000, 0.000000000000000000, 0.000000000000000000 ) ) ;
#5781 = AXIS2_PLACEMENT_3D ( 'NONE', #21052, #19198, #3130 ) ;
#5782 = EDGE_CURVE ( 'NONE', #18497, #9321, #10853, .T. ) ;
#5783 = CARTESIAN_POINT ( 'NONE',  ( 2.000000000000000888, 27.62500000000000000, 12.46410161513774817 ) ) ;
#5784 = CARTESIAN_POINT ( 'NONE',  ( -3.756430356249996994, -8.999999999999992895, 0.4781249993854840286 ) ) ;
#5785 = CYLINDRICAL_SURFACE ( 'NONE', #17629, 1.000000000000000000 ) ;
#5786 = CARTESIAN_POINT ( 'NONE',  ( -3.397863563850083146, -30.85476721088024021, -6.500000000000000000 ) ) ;
#5787 = EDGE_LOOP ( 'NONE', ( #9592, #8354, #12731, #15077 ) ) ;
#5788 = VERTEX_POINT ( 'NONE', #8462 ) ;
#5789 = CARTESIAN_POINT ( 'NONE',  ( 6.009258394948636914E-15, 29.55624999877097636, 4.381197846482986158 ) ) ;
#5790 = EDGE_CURVE ( 'NONE', #13306, #6385, #3504, .T. ) ;
#5792 = ORIENTED_EDGE ( 'NONE', *, *, #21913, .T. ) ;
#5791 = CIRCLE ( 'NONE', #2457, 0.5000000000000006661 ) ;
#5793 = DIRECTION ( 'NONE',  ( 1.000000000000000000, 0.000000000000000000, 0.000000000000000000 ) ) ;
#5794 = CIRCLE ( 'NONE', #19566, 31.10000000000000142 ) ;
#5795 = CARTESIAN_POINT ( 'NONE',  ( 1.859271017917182139E-15, 29.38750000000000639, 12.99999999999999289 ) ) ;
#5796 = DIRECTION ( 'NONE',  ( 0.000000000000000000, 0.000000000000000000, 1.000000000000000000 ) ) ;
#5797 = ORIENTED_EDGE ( 'NONE', *, *, #15047, .T. ) ;
#5798 = ADVANCED_FACE ( 'NONE', ( #14355 ), #10537, .T. ) ;
#5799 = VERTEX_POINT ( 'NONE', #21010 ) ;
#5800 = CIRCLE ( 'NONE', #20835, 0.5000000000000001110 ) ;
#5801 = CARTESIAN_POINT ( 'NONE',  ( 4.000000000000005329, 25.03750000000000497, 6.690598923241489970 ) ) ;
#5802 = VECTOR ( 'NONE', #13084, 1000.000000000000000 ) ;
#5803 = ORIENTED_EDGE ( 'NONE', *, *, #11589, .F. ) ;
#5804 = EDGE_CURVE ( 'NONE', #4455, #1627, #6847, .T. ) ;
#5805 = CARTESIAN_POINT ( 'NONE',  ( 3.110308778861319290, 38.49999999999999289, 3.869115154270335477 ) ) ;
#5806 = CARTESIAN_POINT ( 'NONE',  ( 3.469446951953614189E-15, 30.00000000000000355, 8.999999999999992895 ) ) ;
#5807 = CARTESIAN_POINT ( 'NONE',  ( 3.756430356250004099, 26.90312499938548996, 11.16877607737301403 ) ) ;
#5808 = EDGE_CURVE ( 'NONE', #21834, #3291, #4680, .T. ) ;
#5809 = DIRECTION ( 'NONE',  ( 0.000000000000000000, 0.000000000000000000, 1.000000000000000000 ) ) ;
#5810 = CARTESIAN_POINT ( 'NONE',  ( -3.999999999999999556, 27.43750000000001066, 6.690598923241487306 ) ) ;
#5811 = AXIS2_PLACEMENT_3D ( 'NONE', #2077, #25358, #7440 ) ;
#5812 = CARTESIAN_POINT ( 'NONE',  ( 1.878215178125004048, 26.11562499938548498, 5.746835883940462963 ) ) ;
#5813 = CARTESIAN_POINT ( 'NONE',  ( 4.000000000000003553, -6.690598923241489970, 0.03749999999999697325 ) ) ;
#5814 = AXIS2_PLACEMENT_3D ( 'NONE', #25283, #5397, #9579 ) ;
#5815 = CARTESIAN_POINT ( 'NONE',  ( 2.000000000000000888, -12.46410161513774817, 1.218749998770966902 ) ) ;
#5816 = VECTOR ( 'NONE', #14198, 1000.000000000000000 ) ;
#5817 = CARTESIAN_POINT ( 'NONE',  ( -3.918623196469518177, 38.49999999999999289, 4.456389954662586028 ) ) ;
#5818 = CARTESIAN_POINT ( 'NONE',  ( 20.09951025522764922, 17.27108313048138655, 5.535898384862238508 ) ) ;
#5819 = CARTESIAN_POINT ( 'NONE',  ( 21.35910797434536335, 18.70291059638591946, 12.25316411605952283 ) ) ;
#5820 = CARTESIAN_POINT ( 'NONE',  ( -3.834746474454188013E-15, -28.65624999877096712, 4.999999999999992006 ) ) ;
#5821 = CARTESIAN_POINT ( 'NONE',  ( 2.000000000000000888, 28.07500000000000284, 12.46410161513774817 ) ) ;
#5822 = FACE_OUTER_BOUND ( 'NONE', #12954, .T. ) ;
#5823 = CARTESIAN_POINT ( 'NONE',  ( -8.366719580627318441E-15, 29.55624999877097636, 4.999999999999992006 ) ) ;
#5824 = VECTOR ( 'NONE', #12697, 1000.000000000000000 ) ;
#5825 = DIRECTION ( 'NONE',  ( 0.000000000000000000, -0.000000000000000000, -1.000000000000000000 ) ) ;
#5826 = VERTEX_POINT ( 'NONE', #7139 ) ;
#5827 = CARTESIAN_POINT ( 'NONE',  ( 3.752267015613588906E-15, 27.30624999877097281, 4.381197846482986158 ) ) ;
#5828 = CARTESIAN_POINT ( 'NONE',  ( 3.999999999999996003, -26.53750000000000142, 6.690598923241487306 ) ) ;
#5830 = ORIENTED_EDGE ( 'NONE', *, *, #3597, .F. ) ;
#5829 = CARTESIAN_POINT ( 'NONE',  ( -3.756430356249997882, 25.92812499938548854, 8.999999999999992895 ) ) ;
#5831 = CARTESIAN_POINT ( 'NONE',  ( -1.878215178124995832, 29.45312499938548356, 5.746835883940462963 ) ) ;
#5832 = COLOUR_RGB ( '',0.8941176470588234615, 0.8941176470588234615, 0.8941176470588234615 ) ;
#5833 = CARTESIAN_POINT ( 'NONE',  ( 1.071796769724493448, -29.57634618820329564, 4.999999999999995559 ) ) ;
#5834 = AXIS2_PLACEMENT_3D ( 'NONE', #25451, #9385, #1795 ) ;
#5835 = CARTESIAN_POINT ( 'NONE',  ( -3.403349963601461248, 25.83240171513484285, 20.00001200000000168 ) ) ;
#5836 = CARTESIAN_POINT ( 'NONE',  ( 1.626862140677534194E-14, 28.43124999877096570, 12.99999999999999289 ) ) ;
#5837 = VERTEX_POINT ( 'NONE', #24922 ) ;
#5838 = ORIENTED_EDGE ( 'NONE', *, *, #19516, .T. ) ;
#5839 = ADVANCED_FACE ( 'NONE', ( #5563 ), #21392, .T. ) ;
#5840 = CARTESIAN_POINT ( 'NONE',  ( -2.003086131649545506E-15, 26.37812499938548427, 13.33755215474602984 ) ) ;
#5842 = EDGE_CURVE ( 'NONE', #10320, #7996, #19289, .T. ) ;
#5841 = COLOUR_RGB ( '',0.8941176470588234615, 0.8941176470588234615, 0.8941176470588234615 ) ;
#5843 = AXIS2_PLACEMENT_3D ( 'NONE', #3168, #18732, #23057 ) ;
#5844 = CARTESIAN_POINT ( 'NONE',  ( -1.878215178124998497, -12.25316411605951927, 4.040624999385483918 ) ) ;
#5845 = EDGE_CURVE ( 'NONE', #19280, #14695, #15249, .T. ) ;
#5846 = VECTOR ( 'NONE', #23777, 1000.000000000000000 ) ;
#5847 = CARTESIAN_POINT ( 'NONE',  ( -1.071796769724485232, 28.22634618820330132, 4.999999999999992006 ) ) ;
#5848 = CARTESIAN_POINT ( 'NONE',  ( 3.959305671612554781E-15, 35.50000000000000711, 12.99999999999999289 ) ) ;
#5849 = VECTOR ( 'NONE', #17437, 1000.000000000000000 ) ;
#5850 = CARTESIAN_POINT ( 'NONE',  ( -1.452785157361865531, -31.03863125411923463, 1.000000000000000000 ) ) ;
#5851 = CARTESIAN_POINT ( 'NONE',  ( 1.071796769724490561, 29.53615380933863577, 4.999999999999988454 ) ) ;
#5852 = CARTESIAN_POINT ( 'NONE',  ( 5.706339097770919189, 29.50000000000000000, 7.645898033750285983 ) ) ;
#5853 = CARTESIAN_POINT ( 'NONE',  ( 19.23330444827413643, 22.06173157302024634, 5.535898384862237620 ) ) ;
#5854 = CYLINDRICAL_SURFACE ( 'NONE', #24175, 4.000000000000000000 ) ;
#5855 = FACE_OUTER_BOUND ( 'NONE', #290, .T. ) ;
#5856 = ORIENTED_EDGE ( 'NONE', *, *, #12211, .F. ) ;
#5857 = CYLINDRICAL_SURFACE ( 'NONE', #9697, 0.5000000000000004441 ) ;
#5858 = CARTESIAN_POINT ( 'NONE',  ( 5.485456488530129349, 38.54977203910393513, 6.694575048425325470 ) ) ;
#5859 = CARTESIAN_POINT ( 'NONE',  ( -3.756430356249995661, 27.69062499938548427, 6.831223922626973533 ) ) ;
#5860 = VECTOR ( 'NONE', #3539, 1000.000000000000000 ) ;
#5861 = PLANE ( 'NONE',  #24166 ) ;
#5862 = DIRECTION ( 'NONE',  ( 1.000000000000000000, 0.000000000000000000, 0.000000000000000000 ) ) ;
#5863 = DIRECTION ( 'NONE',  ( 0.000000000000000000, 0.000000000000000000, 1.000000000000000000 ) ) ;
#5864 = ORIENTED_EDGE ( 'NONE', *, *, #14835, .F. ) ;
#5865 = CARTESIAN_POINT ( 'NONE',  ( 4.000000000000003553, 26.74374999877097281, 8.999999999999992895 ) ) ;
#5866 = CARTESIAN_POINT ( 'NONE',  ( -3.756430356250004099, -25.17812499938548498, 6.831223922626973533 ) ) ;
#5868 = ORIENTED_EDGE ( 'NONE', *, *, #11059, .F. ) ;
#5867 = CARTESIAN_POINT ( 'NONE',  ( 1.500000000000001776, -10.49999999999999289, 30.00000000000000355 ) ) ;
#5869 = ORIENTED_EDGE ( 'NONE', *, *, #22549, .T. ) ;
#5870 = VECTOR ( 'NONE', #22003, 1000.000000000000000 ) ;
#5871 = VERTEX_POINT ( 'NONE', #3472 ) ;
#5872 = VERTEX_POINT ( 'NONE', #13031 ) ;
#5873 = ORIENTED_EDGE ( 'NONE', *, *, #7331, .T. ) ;
#5874 = FACE_OUTER_BOUND ( 'NONE', #3360, .T. ) ;
#5875 = DIRECTION ( 'NONE',  ( -0.000000000000000000, -1.000000000000000000, -0.000000000000000000 ) ) ;
#5876 = EDGE_CURVE ( 'NONE', #4812, #9189, #24799, .T. ) ;
#5877 = CIRCLE ( 'NONE', #21745, 31.10000000000000142 ) ;
#5878 = CARTESIAN_POINT ( 'NONE',  ( 0.7500000000000001110, 0.000000000000000000, 17.00000000000000000 ) ) ;
#5879 = AXIS2_PLACEMENT_3D ( 'NONE', #15777, #4653, #12635 ) ;
#5880 = CARTESIAN_POINT ( 'NONE',  ( -3.756430356249996105, 27.57812499938548356, 6.831223922626973533 ) ) ;
#5881 = VECTOR ( 'NONE', #13871, 1000.000000000000000 ) ;
#5882 = CARTESIAN_POINT ( 'NONE',  ( -1.878215178124995832, -5.746835883940462963, 1.640624999385484450 ) ) ;
#5883 = CARTESIAN_POINT ( 'NONE',  ( 2.620986760973688460E-15, -13.61880215351699874, 3.881249998770965437 ) ) ;
#5884 =( NAMED_UNIT ( * ) SI_UNIT ( $, .STERADIAN. ) SOLID_ANGLE_UNIT ( ) );
#5885 = CARTESIAN_POINT ( 'NONE',  ( -3.756430356249996994, 28.17812499938548498, 8.999999999999992895 ) ) ;
#5886 = EDGE_CURVE ( 'NONE', #7162, #12485, #1002, .T. ) ;
#5887 = DIRECTION ( 'NONE',  ( 0.3090169943749591086, 0.9510565162951497564, 0.000000000000000000 ) ) ;
#5888 = CARTESIAN_POINT ( 'NONE',  ( -1.999999999999998224, -12.46410161513774639, 1.593749998770967125 ) ) ;
#5889 = CARTESIAN_POINT ( 'NONE',  ( 2.620986760973688460E-15, -13.61880215351699874, 1.687500000000000000 ) ) ;
#5890 = DIRECTION ( 'NONE',  ( -0.000000000000000000, -1.000000000000000000, -0.000000000000000000 ) ) ;
#5891 = PLANE ( 'NONE',  #25816 ) ;
#5892 = CARTESIAN_POINT ( 'NONE',  ( 5.577813053751546416E-15, 27.81250000000000355, 4.999999999999992006 ) ) ;
#5893 = CARTESIAN_POINT ( 'NONE',  ( -4.000000000000003553, -29.48124999877096997, 6.690598923241489970 ) ) ;
#5894 = CARTESIAN_POINT ( 'NONE',  ( -1.878215178124995832, 27.20312499938548711, 5.746835883940462963 ) ) ;
#5895 = DIRECTION ( 'NONE',  ( -0.000000000000000000, -0.000000000000000000, 1.000000000000000000 ) ) ;
#5896 = CARTESIAN_POINT ( 'NONE',  ( 4.000000000000005329, 28.09374999877097778, 8.999999999999992895 ) ) ;
#5897 = CARTESIAN_POINT ( 'NONE',  ( 1.071796769724488563, -26.16115380933863221, 12.99999999999999289 ) ) ;
#5898 = ORIENTED_EDGE ( 'NONE', *, *, #24116, .F. ) ;
#5899 = CARTESIAN_POINT ( 'NONE',  ( -1.071796769724486564, 27.11740381056766935, 12.99999999999999467 ) ) ;
#5901 = ORIENTED_EDGE ( 'NONE', *, *, #7980, .T. ) ;
#5900 = CARTESIAN_POINT ( 'NONE',  ( 4.000000000000003553, 28.15000000000000213, 8.999999999999992895 ) ) ;
#5902 = VECTOR ( 'NONE', #22321, 1000.000000000000000 ) ;
#5903 = ORIENTED_EDGE ( 'NONE', *, *, #2796, .T. ) ;
#5904 = DIRECTION ( 'NONE',  ( 0.000000000000000000, 0.000000000000000000, 1.000000000000000000 ) ) ;
#5905 = VERTEX_POINT ( 'NONE', #1510 ) ;
#5906 = CARTESIAN_POINT ( 'NONE',  ( -1.878215178125000939, -28.32812499938548711, 12.25316411605952283 ) ) ;
#5907 = ORIENTED_EDGE ( 'NONE', *, *, #21594, .F. ) ;
#5908 = CARTESIAN_POINT ( 'NONE',  ( 3.469446951953614189E-15, 35.50000000000000711, 8.999999999999992895 ) ) ;
#5909 = CIRCLE ( 'NONE', #17198, 1.500000000000000222 ) ;
#5910 = ORIENTED_EDGE ( 'NONE', *, *, #8610, .F. ) ;
#5911 = CARTESIAN_POINT ( 'NONE',  ( -1.999999999999998224, 28.90000000000000213, 12.46410161513774639 ) ) ;
#5912 = CARTESIAN_POINT ( 'NONE',  ( -3.756430356249996994, 26.82812499938548711, 8.999999999999992895 ) ) ;
#5913 = VECTOR ( 'NONE', #10901, 1000.000000000000000 ) ;
#5914 = AXIS2_PLACEMENT_3D ( 'NONE', #22663, #20690, #18720 ) ;
#5915 = EDGE_CURVE ( 'NONE', #7097, #23080, #14984, .T. ) ;
#5916 = CARTESIAN_POINT ( 'NONE',  ( 3.735045420075836212E-15, -4.662447845253954171, 0.8156249993854834957 ) ) ;
#5917 = CARTESIAN_POINT ( 'NONE',  ( 21.21320343559646915, 21.21320343559638744, 12.99999999999999289 ) ) ;
#5918 = CARTESIAN_POINT ( 'NONE',  ( 20.95908693567302450, 20.95908693567294989, 13.33755215474602984 ) ) ;
#5919 = AXIS2_PLACEMENT_3D ( 'NONE', #15642, #11703, #19682 ) ;
#5920 = DIRECTION ( 'NONE',  ( 0.000000000000000000, 0.000000000000000000, -1.000000000000000000 ) ) ;
#5921 = DIRECTION ( 'NONE',  ( -0.000000000000000000, -1.000000000000000000, -0.000000000000000000 ) ) ;
#5922 = ITEM_DEFINED_TRANSFORMATION ( 'NONE', 'NONE', #25251,  #21036 ) ;
#5923 = CARTESIAN_POINT ( 'NONE',  ( 4.000000000000003553, 28.63750000000000284, 6.690598923241489970 ) ) ;
#5924 = EDGE_CURVE ( 'NONE', #15245, #15811, #23550, .T. ) ;
#5925 = DIRECTION ( 'NONE',  ( 1.000000000000000000, 0.000000000000000000, 0.000000000000000000 ) ) ;
#5926 = DIRECTION ( 'NONE',  ( 1.000000000000000000, 0.000000000000000000, 0.000000000000000000 ) ) ;
#5927 = DIRECTION ( 'NONE',  ( 0.000000000000000000, 0.000000000000000000, 1.000000000000000000 ) ) ;
#5928 = ORIENTED_EDGE ( 'NONE', *, *, #19790, .T. ) ;
#5929 = VERTEX_POINT ( 'NONE', #3203 ) ;
#5930 = CARTESIAN_POINT ( 'NONE',  ( 6.009258394948636914E-15, 26.26562499938548356, 4.662447845253954171 ) ) ;
#5931 = AXIS2_PLACEMENT_3D ( 'NONE', #23799, #24184, #25761 ) ;
#5932 = AXIS2_PLACEMENT_3D ( 'NONE', #7846, #13498, #25646 ) ;
#5933 = ORIENTED_EDGE ( 'NONE', *, *, #14498, .T. ) ;
#5934 = CARTESIAN_POINT ( 'NONE',  ( 19.62663259444009611, 19.62663259444001440, 4.999999999999992006 ) ) ;
#5935 = CARTESIAN_POINT ( 'NONE',  ( 1.878215178125004048, 25.32812499938548356, 5.746835883940462963 ) ) ;
#5936 = CARTESIAN_POINT ( 'NONE',  ( 3.756430356250002323, 29.26562499938548356, 11.16877607737301226 ) ) ;
#5937 = CARTESIAN_POINT ( 'NONE',  ( 16.47558800164659587, 19.30401512639272354, 12.46410161513774639 ) ) ;
#5938 = VERTEX_POINT ( 'NONE', #25428 ) ;
#5939 = ORIENTED_EDGE ( 'NONE', *, *, #24006, .F. ) ;
#5940 = CIRCLE ( 'NONE', #6784, 31.10000000000000142 ) ;
#5941 = CARTESIAN_POINT ( 'NONE',  ( 1.500000000000001776, -7.499999999999993783, 4.999999999999993783 ) ) ;
#5942 = VERTEX_POINT ( 'NONE', #25189 ) ;
#5943 = DIRECTION ( 'NONE',  ( -1.000000000000000000, 0.000000000000000000, 0.000000000000000000 ) ) ;
#5944 = CARTESIAN_POINT ( 'NONE',  ( -3.756430356249995661, 27.12812499938548427, 6.831223922626973533 ) ) ;
#5945 =( BOUNDED_CURVE ( )  B_SPLINE_CURVE ( 2, ( #24361, #570, #2513, #20689, #22662, #6439, #22385, #10732, #18719 ),
 .UNSPECIFIED., .F., .F. ) 
 B_SPLINE_CURVE_WITH_KNOTS ( ( 3, 2, 2, 2, 3 ),
 ( 0.5250000000000000222, 0.5333333333333333259, 0.5500000000000000444, 0.5666666666666666519, 0.5750000000000000666 ),
 .UNSPECIFIED. ) 
 CURVE ( )  GEOMETRIC_REPRESENTATION_ITEM ( )  RATIONAL_B_SPLINE_CURVE ( ( 0.9330127018922194093, 0.9330127018922194093, 1.000000000000000000, 0.8660254037844387076, 1.000000000000000000, 0.8660254037844387076, 1.000000000000000000, 0.9330127018922189652, 0.9330127018922194093 ) ) 
 REPRESENTATION_ITEM ( '' )  );
#5946 = CARTESIAN_POINT ( 'NONE',  ( 3.756430356250006319, 26.97812499938547859, 6.831223922626973533 ) ) ;
#5947 = DIRECTION ( 'NONE',  ( 1.000000000000000000, 0.000000000000000000, 0.000000000000000000 ) ) ;
#5948 = FACE_OUTER_BOUND ( 'NONE', #1696, .T. ) ;
#5949 = CARTESIAN_POINT ( 'NONE',  ( 4.000000000000000888, 28.11250000000000426, 11.30940107675849760 ) ) ;
#5950 = EDGE_CURVE ( 'NONE', #15046, #13062, #11023, .T. ) ;
#5951 = CARTESIAN_POINT ( 'NONE',  ( 3.756430356250004099, 25.62812499938548072, 6.831223922626973533 ) ) ;
#5952 = EDGE_CURVE ( 'NONE', #6478, #6543, #7682, .T. ) ;
#5953 = CARTESIAN_POINT ( 'NONE',  ( 3.752267015613588906E-15, -4.381197846482986158, 0.1124999999999989203 ) ) ;
#5954 = CARTESIAN_POINT ( 'NONE',  ( -1.999999999999995781, 27.40000000000000213, 5.535898384862237620 ) ) ;
#5955 = FACE_OUTER_BOUND ( 'NONE', #16589, .T. ) ;
#5956 = CARTESIAN_POINT ( 'NONE',  ( 22.75999951944203303, 17.10314526994957873, 6.690598923241489970 ) ) ;
#5957 = CARTESIAN_POINT ( 'NONE',  ( 3.959305671612554781E-15, 40.00000000000000000, 12.99999999999999289 ) ) ;
#5958 = EDGE_CURVE ( 'NONE', #930, #17209, #15126, .T. ) ;
#5959 = CARTESIAN_POINT ( 'NONE',  ( 2.000000000000003997, -5.535898384862238508, 4.518749998770967835 ) ) ;
#5960 = CARTESIAN_POINT ( 'NONE',  ( 29.99470236596026496, -8.217531866531315288, -6.500000000000000000 ) ) ;
#5961 = CARTESIAN_POINT ( 'NONE',  ( -3.999999999999996447, 25.22500000000000142, 8.999999999999992895 ) ) ;
#5962 = MECHANICAL_DESIGN_GEOMETRIC_PRESENTATION_REPRESENTATION (  '', ( #18080 ), #3870 ) ;
#5963 = CARTESIAN_POINT ( 'NONE',  ( -24.27856662945521649, -19.43607991388963185, -2.750000000000000000 ) ) ;
#5964 = ORIENTED_EDGE ( 'NONE', *, *, #3925, .T. ) ;
#5965 = CARTESIAN_POINT ( 'NONE',  ( 4.000000000000001776, 27.15624999877097423, 11.30940107675849760 ) ) ;
#5966 = CARTESIAN_POINT ( 'NONE',  ( 3.999999999999997335, -27.51250000000000284, 11.30940107675849404 ) ) ;
#5968 = ORIENTED_EDGE ( 'NONE', *, *, #21128, .T. ) ;
#5967 = CARTESIAN_POINT ( 'NONE',  ( 6.009258394948636914E-15, 26.26562499938548356, 4.662447845253954171 ) ) ;
#5969 = CARTESIAN_POINT ( 'NONE',  ( -3.756430356249996105, 29.04062499938548569, 6.831223922626973533 ) ) ;
#5970 = DIRECTION ( 'NONE',  ( -0.9822872507286897203, -0.1873813145857189666, 0.000000000000000000 ) ) ;
#5971 = DIRECTION ( 'NONE',  ( -0.000000000000000000, -0.000000000000000000, -1.000000000000000000 ) ) ;
#5972 = CARTESIAN_POINT ( 'NONE',  ( -24.00000000000000355, 2.939152317953648289E-15, 17.00000000000000000 ) ) ;
#5973 = ORIENTED_EDGE ( 'NONE', *, *, #23660, .T. ) ;
#5974 = VERTEX_POINT ( 'NONE', #15509 ) ;
#5975 = DIRECTION ( 'NONE',  ( 0.000000000000000000, 1.000000000000000000, 0.000000000000000000 ) ) ;
#5976 = CARTESIAN_POINT ( 'NONE',  ( 6.009258394948636914E-15, 26.60312499938547859, 4.662447845253954171 ) ) ;
#5977 = CIRCLE ( 'NONE', #5550, 31.10000000000000142 ) ;
#5978 = ADVANCED_BREP_SHAPE_REPRESENTATION ( '', ( #4802, #21036 ), #5183 ) ;
#5979 = CARTESIAN_POINT ( 'NONE',  ( 3.756430356250003655, -8.999999999999992895, 3.290624999385483029 ) ) ;
#5980 = AXIS2_PLACEMENT_3D ( 'NONE', #14052, #66, #16022 ) ;
#5981 = CARTESIAN_POINT ( 'NONE',  ( 3.469446951953614189E-15, 31.50000000000000000, 8.999999999999992895 ) ) ;
#5982 = DIRECTION ( 'NONE',  ( -0.000000000000000000, -0.000000000000000000, -1.000000000000000000 ) ) ;
#5983 = PLANE ( 'NONE',  #22192 ) ;
#5984 = DIRECTION ( 'NONE',  ( 0.000000000000000000, 0.000000000000000000, -1.000000000000000000 ) ) ;
#5985 = CARTESIAN_POINT ( 'NONE',  ( -1.999999999999994893, 26.44374999877097210, 5.535898384862237620 ) ) ;
#5986 = DIRECTION ( 'NONE',  ( 0.000000000000000000, 1.000000000000000000, 0.000000000000000000 ) ) ;
#5987 = CARTESIAN_POINT ( 'NONE',  ( 18.51293941407127619, 18.51293941407120869, 13.61880215351699874 ) ) ;
#5988 = EDGE_CURVE ( 'NONE', #20014, #8256, #7354, .T. ) ;
#5989 = VERTEX_POINT ( 'NONE', #19802 ) ;
#5990 = CARTESIAN_POINT ( 'NONE',  ( 4.393401135980900207, -30.78811501957146390, -6.500000000000000000 ) ) ;
#5991 = CARTESIAN_POINT ( 'NONE',  ( -24.00000000000000355, 2.939152317953648289E-15, 17.00000000000000000 ) ) ;
#5992 = CARTESIAN_POINT ( 'NONE',  ( 3.756430356250002323, 27.91562499938548569, 11.16877607737301226 ) ) ;
#5993 = EDGE_CURVE ( 'NONE', #789, #15159, #16355, .T. ) ;
#5994 = DIRECTION ( 'NONE',  ( -0.000000000000000000, 1.000000000000000000, -0.000000000000000000 ) ) ;
#5995 = MECHANICAL_DESIGN_GEOMETRIC_PRESENTATION_REPRESENTATION (  '', ( #8922 ), #15605 ) ;
#5996 = CARTESIAN_POINT ( 'NONE',  ( -3.999999999999995559, 26.48124999877096641, 6.690598923241487306 ) ) ;
#5997 = DIRECTION ( 'NONE',  ( -0.000000000000000000, -1.000000000000000000, -0.000000000000000000 ) ) ;
#5998 = ORIENTED_EDGE ( 'NONE', *, *, #431, .F. ) ;
#5999 = CARTESIAN_POINT ( 'NONE',  ( 3.834746474454188013E-15, 25.56250000000000000, 4.999999999999992006 ) ) ;
#6000 = CARTESIAN_POINT ( 'NONE',  ( 4.000000000000003553, 29.50000000000000355, 8.999999999999992895 ) ) ;
#6001 = CARTESIAN_POINT ( 'NONE',  ( -14.48253926456298579, 27.25313774936435962, -6.500000000000000000 ) ) ;
#6003 = ORIENTED_EDGE ( 'NONE', *, *, #9000, .F. ) ;
#6002 = DIRECTION ( 'NONE',  ( 0.000000000000000000, 0.000000000000000000, 1.000000000000000000 ) ) ;
#6004 = AXIS2_PLACEMENT_3D ( 'NONE', #24558, #10962, #18815 ) ;
#6005 = EDGE_LOOP ( 'NONE', ( #19144, #3901, #2015, #17719, #4425, #25355, #24586, #6246 ) ) ;
#6006 = ORIENTED_EDGE ( 'NONE', *, *, #25353, .T. ) ;
#6007 = ORIENTED_EDGE ( 'NONE', *, *, #6490, .T. ) ;
#6008 = DIRECTION ( 'NONE',  ( -0.7071067811865487940, -0.7071067811865463515, 0.000000000000000000 ) ) ;
#6009 = CARTESIAN_POINT ( 'NONE',  ( -3.023184356956651442, 38.77026726007181878, 13.86739978446106392 ) ) ;
#6010 = CYLINDRICAL_SURFACE ( 'NONE', #18538, 8.000000000000000000 ) ;
#6011 = CARTESIAN_POINT ( 'NONE',  ( 3.756430356250004543, 26.90312499938548996, 11.16877607737301226 ) ) ;
#6012 =( GEOMETRIC_REPRESENTATION_CONTEXT ( 3 ) GLOBAL_UNCERTAINTY_ASSIGNED_CONTEXT ( ( #2860 ) ) GLOBAL_UNIT_ASSIGNED_CONTEXT ( ( #7555, #15405, #3626 ) ) REPRESENTATION_CONTEXT ( 'NONE', 'WORKASPACE' ) );
#6013 = CARTESIAN_POINT ( 'NONE',  ( -3.756430356249996994, -8.999999999999992895, 2.165624999385482141 ) ) ;
#6014 = CARTESIAN_POINT ( 'NONE',  ( 3.752267015613588906E-15, -4.381197846482986158, 4.106249998770966414 ) ) ;
#6015 =( NAMED_UNIT ( * ) SI_UNIT ( $, .STERADIAN. ) SOLID_ANGLE_UNIT ( ) );
#6016 = CARTESIAN_POINT ( 'NONE',  ( -1.878215178124998497, 28.70312499938548356, 12.25316411605951927 ) ) ;
#6017 = PLANE ( 'NONE',  #14666 ) ;
#6018 = DIRECTION ( 'NONE',  ( 1.000000000000000000, 0.000000000000000000, 0.000000000000000000 ) ) ;
#6019 = EDGE_CURVE ( 'NONE', #10563, #12702, #12156, .T. ) ;
#6020 = CARTESIAN_POINT ( 'NONE',  ( 3.756430356250003211, 26.52812499938548285, 6.831223922626973533 ) ) ;
#6021 = FACE_OUTER_BOUND ( 'NONE', #23857, .T. ) ;
#6022 = DIRECTION ( 'NONE',  ( 0.000000000000000000, 0.000000000000000000, 1.000000000000000000 ) ) ;
#6023 = CARTESIAN_POINT ( 'NONE',  ( 0.000000000000000000, 0.000000000000000000, -6.500000000000000000 ) ) ;
#6024 = CARTESIAN_POINT ( 'NONE',  ( -1.878215178125004048, -25.32812499938548356, 5.746835883940462963 ) ) ;
#6025 = CARTESIAN_POINT ( 'NONE',  ( -3.756430356249997882, 28.21562499938548285, 11.16877607737301226 ) ) ;
#6026 = EDGE_CURVE ( 'NONE', #22395, #12276, #11548, .T. ) ;
#6027 = DIRECTION ( 'NONE',  ( 0.000000000000000000, 0.000000000000000000, 1.000000000000000000 ) ) ;
#6028 = CARTESIAN_POINT ( 'NONE',  ( 0.000000000000000000, 0.000000000000000000, 19.00000000000000000 ) ) ;
#6029 = VERTEX_POINT ( 'NONE', #23990 ) ;
#6030 = CARTESIAN_POINT ( 'NONE',  ( 25.99307600111999150, -0.5999999999999996447, 19.59999999999999787 ) ) ;
#6032 = ORIENTED_EDGE ( 'NONE', *, *, #13540, .T. ) ;
#6031 = CARTESIAN_POINT ( 'NONE',  ( -2.672651547586948120E-15, -29.07812499938548356, 13.33755215474603162 ) ) ;
#6033 = VERTEX_POINT ( 'NONE', #11948 ) ;
#6034 = FACE_OUTER_BOUND ( 'NONE', #16107, .T. ) ;
#6035 = PRODUCT_DEFINITION_FORMATION_WITH_SPECIFIED_SOURCE ( 'ANY', '', #24254, .NOT_KNOWN. ) ;
#6036 = VERTEX_POINT ( 'NONE', #8044 ) ;
#6037 = ORIENTED_EDGE ( 'NONE', *, *, #344, .T. ) ;
#6038 = ORIENTED_EDGE ( 'NONE', *, *, #7428, .F. ) ;
#6039 = CYLINDRICAL_SURFACE ( 'NONE', #6354, 0.5000000000000004441 ) ;
#6040 = AXIS2_PLACEMENT_3D ( 'NONE', #23259, #17386, #17130 ) ;
#6041 = EDGE_CURVE ( 'NONE', #5355, #311, #5909, .T. ) ;
#6042 = ORIENTED_EDGE ( 'NONE', *, *, #12864, .T. ) ;
#6043 = CARTESIAN_POINT ( 'NONE',  ( 4.000000000000001776, 29.46250000000000568, 11.30940107675849760 ) ) ;
#6044 = CARTESIAN_POINT ( 'NONE',  ( 1.878215178125004048, 27.57812499938548711, 5.746835883940462963 ) ) ;
#6045 = FACE_OUTER_BOUND ( 'NONE', #24408, .T. ) ;
#6046 = CARTESIAN_POINT ( 'NONE',  ( 1.071796769724490783, 25.80759618943233846, 12.99999999999999467 ) ) ;
#6047 = CARTESIAN_POINT ( 'NONE',  ( 18.46426205773553164, 21.12045943569482986, 5.746835883940462963 ) ) ;
#6048 = FACE_OUTER_BOUND ( 'NONE', #12432, .T. ) ;
#6049 = PLANE ( 'NONE',  #8799 ) ;
#6050 =( NAMED_UNIT ( * ) SI_UNIT ( $, .STERADIAN. ) SOLID_ANGLE_UNIT ( ) );
#6051 = CARTESIAN_POINT ( 'NONE',  ( 3.752267015613588906E-15, 28.71250000000000568, 4.381197846482986158 ) ) ;
#6052 = EDGE_CURVE ( 'NONE', #18040, #7266, #24692, .T. ) ;
#6053 = CARTESIAN_POINT ( 'NONE',  ( -3.999999999999995559, 29.23750000000000071, 6.690598923241487306 ) ) ;
#6054 = CARTESIAN_POINT ( 'NONE',  ( 20.95908693567301739, 20.95908693567294989, 13.33755215474603162 ) ) ;
#6055 = LINE ( 'NONE', #5786, #11165 ) ;
#6056 = ORIENTED_EDGE ( 'NONE', *, *, #579, .T. ) ;
#6057 = ORIENTED_EDGE ( 'NONE', *, *, #22318, .F. ) ;
#6058 = CARTESIAN_POINT ( 'NONE',  ( -1.878215178124999829, 26.45312499938549422, 12.25316411605951927 ) ) ;
#6059 = ADVANCED_FACE ( 'NONE', ( #9610 ), #6072, .F. ) ;
#6060 = ORIENTED_EDGE ( 'NONE', *, *, #7451, .T. ) ;
#6061 = FACE_OUTER_BOUND ( 'NONE', #3393, .T. ) ;
#6062 = CARTESIAN_POINT ( 'NONE',  ( 4.000000000000001776, 29.85624999877096997, 11.30940107675849760 ) ) ;
#6063 = CARTESIAN_POINT ( 'NONE',  ( -1.878215178124998497, 29.60312499938548569, 12.25316411605951927 ) ) ;
#6064 = CARTESIAN_POINT ( 'NONE',  ( 0.000000000000000000, 20.00000000000000000, 17.69999999999999929 ) ) ;
#6065 = ORIENTED_EDGE ( 'NONE', *, *, #12246, .T. ) ;
#6066 = EDGE_CURVE ( 'NONE', #19703, #7733, #25569, .T. ) ;
#6067 = CARTESIAN_POINT ( 'NONE',  ( 1.999999999999998224, -25.75000000000000355, 12.46410161513774639 ) ) ;
#6068 = ORIENTED_EDGE ( 'NONE', *, *, #3082, .T. ) ;
#6069 = DIRECTION ( 'NONE',  ( 0.000000000000000000, 0.000000000000000000, -1.000000000000000000 ) ) ;
#6070 = CARTESIAN_POINT ( 'NONE',  ( -3.756430356249995661, 27.57812499938548356, 6.831223922626973533 ) ) ;
#6071 = CARTESIAN_POINT ( 'NONE',  ( -1.878215178124998275, 29.49062499938548854, 12.25316411605951927 ) ) ;
#6072 = CYLINDRICAL_SURFACE ( 'NONE', #4635, 4.000000000000000000 ) ;
#6073 = DIRECTION ( 'NONE',  ( 1.000000000000000000, 0.000000000000000000, 0.000000000000000000 ) ) ;
#6074 = CARTESIAN_POINT ( 'NONE',  ( 4.006172263299091013E-15, 29.16250000000000497, 4.381197846482986158 ) ) ;
#6075 = LINE ( 'NONE', #14058, #13855 ) ;
#6076 = DIRECTION ( 'NONE',  ( 1.000000000000000000, 0.000000000000000000, 0.000000000000000000 ) ) ;
#6077 = CARTESIAN_POINT ( 'NONE',  ( 19.50730832598391729, 19.50730832598384623, 13.61880215351699874 ) ) ;
#6078 = CARTESIAN_POINT ( 'NONE',  ( -31.06601413805600842, 1.453535542772947942, -2.750000000000000000 ) ) ;
#6079 = FACE_OUTER_BOUND ( 'NONE', #18000, .T. ) ;
#6080 =( BOUNDED_CURVE ( )  B_SPLINE_CURVE ( 2, ( #17579, #57, #9976, #9469, #7885 ),
 .UNSPECIFIED., .F., .F. ) 
 B_SPLINE_CURVE_WITH_KNOTS ( ( 3, 2, 3 ),
 ( 0.9749999999999999778, 0.9833333333333332815, 1.000000000000000000 ),
 .UNSPECIFIED. ) 
 CURVE ( )  GEOMETRIC_REPRESENTATION_ITEM ( )  RATIONAL_B_SPLINE_CURVE ( ( 0.9330127018922194093, 0.9330127018922194093, 1.000000000000000000, 0.8660254037844387076, 1.000000000000000000 ) ) 
 REPRESENTATION_ITEM ( '' )  );
#6081 = CARTESIAN_POINT ( 'NONE',  ( 22.98538980507618845, 17.32853555558373060, 11.30940107675849760 ) ) ;
#6082 = CARTESIAN_POINT ( 'NONE',  ( -21.28941499438242246, -22.67092431280570963, -6.500000000000000000 ) ) ;
#6083 = EDGE_CURVE ( 'NONE', #7895, #933, #13546, .T. ) ;
#6084 = CARTESIAN_POINT ( 'NONE',  ( 21.70382253017380592, 19.04762515221435493, 5.746835883940462963 ) ) ;
#6085 = ORIENTED_EDGE ( 'NONE', *, *, #24897, .T. ) ;
#6086 = CARTESIAN_POINT ( 'NONE',  ( -1.999999999999995781, 27.34374999877097068, 5.535898384862237620 ) ) ;
#6087 = CARTESIAN_POINT ( 'NONE',  ( -3.999999999999996447, -8.999999999999992895, 18.00000000000000000 ) ) ;
#6089 = ORIENTED_EDGE ( 'NONE', *, *, #17341, .F. ) ;
#6088 = CARTESIAN_POINT ( 'NONE',  ( 1.878215178124999829, 26.97812499938549280, 12.25316411605952283 ) ) ;
#6090 = CARTESIAN_POINT ( 'NONE',  ( 3.735045420075836212E-15, 28.06562499938548427, 4.662447845253954171 ) ) ;
#6091 =( BOUNDED_CURVE ( )  B_SPLINE_CURVE ( 2, ( #16063, #4404, #5853, #10030, #18273, #4018, #19836, #16319, #14363 ),
 .UNSPECIFIED., .F., .F. ) 
 B_SPLINE_CURVE_WITH_KNOTS ( ( 3, 2, 2, 2, 3 ),
 ( 0.9250000000000000444, 0.9333333333333333481, 0.9499999999999999556, 0.9666666666666666741, 0.9749999999999999778 ),
 .UNSPECIFIED. ) 
 CURVE ( )  GEOMETRIC_REPRESENTATION_ITEM ( )  RATIONAL_B_SPLINE_CURVE ( ( 0.9330127018922194093, 0.9330127018922198534, 1.000000000000000000, 0.8660254037844387076, 1.000000000000000000, 0.8660254037844387076, 1.000000000000000000, 0.9330127018922194093, 0.9330127018922194093 ) ) 
 REPRESENTATION_ITEM ( '' )  );
#6092 = ADVANCED_FACE ( 'NONE', ( #25817 ), #17981, .T. ) ;
#6093 = DIRECTION ( 'NONE',  ( 0.000000000000000000, 0.000000000000000000, 1.000000000000000000 ) ) ;
#6094 = DIRECTION ( 'NONE',  ( -0.000000000000000000, -0.000000000000000000, 1.000000000000000000 ) ) ;
#6095 = EDGE_LOOP ( 'NONE', ( #11373, #18842, #4902, #21374 ) ) ;
#6096 = ORIENTED_EDGE ( 'NONE', *, *, #25170, .T. ) ;
#6097 = CARTESIAN_POINT ( 'NONE',  ( 3.756430356249996105, -25.44062499938548427, 6.831223922626973533 ) ) ;
#6098 = CARTESIAN_POINT ( 'NONE',  ( 3.756430356250004543, 26.90312499938548996, 11.16877607737301226 ) ) ;
#6099 = CARTESIAN_POINT ( 'NONE',  ( 3.959305739469038251E-15, 30.00000000000000355, 12.99999999999999289 ) ) ;
#6100 = CARTESIAN_POINT ( 'NONE',  ( -3.756430356249996105, -6.831223922626973533, 2.128124999385481608 ) ) ;
#6101 = ADVANCED_FACE ( 'NONE', ( #17724 ), #3591, .T. ) ;
#6102 = DIRECTION ( 'NONE',  ( 0.000000000000000000, -1.000000000000000000, 0.000000000000000000 ) ) ;
#6103 =( NAMED_UNIT ( * ) PLANE_ANGLE_UNIT ( ) SI_UNIT ( $, .RADIAN. ) );
#6104 = FACE_OUTER_BOUND ( 'NONE', #13514, .T. ) ;
#6105 = CYLINDRICAL_SURFACE ( 'NONE', #24679, 31.10000000000000142 ) ;
#6106 = CARTESIAN_POINT ( 'NONE',  ( -0.5000000000000001110, 0.000000000000000000, 20.00000000000000000 ) ) ;
#6107 = CARTESIAN_POINT ( 'NONE',  ( 20.82429470594385634, 15.16744045645140915, 8.999999999999992895 ) ) ;
#6108 = CARTESIAN_POINT ( 'NONE',  ( -3.999999999999996447, 26.55624999877097281, 11.30940107675849404 ) ) ;
#6110 = EDGE_CURVE ( 'NONE', #4583, #3323, #6318, .T. ) ;
#6109 = DIRECTION ( 'NONE',  ( 1.000000000000000000, 0.000000000000000000, 0.000000000000000000 ) ) ;
#6111 = CARTESIAN_POINT ( 'NONE',  ( 16.87775498257738960, 22.53460923206970179, 8.999999999999992895 ) ) ;
#6112 = ORIENTED_EDGE ( 'NONE', *, *, #23921, .F. ) ;
#6113 = CARTESIAN_POINT ( 'NONE',  ( 3.137519842735244810E-15, -26.91249999999999787, 4.999999999999991118 ) ) ;
#6114 = DIRECTION ( 'NONE',  ( 0.000000000000000000, 0.000000000000000000, 1.000000000000000000 ) ) ;
#6115 = CARTESIAN_POINT ( 'NONE',  ( -1.878215178124995832, 29.45312499938548356, 5.746835883940462963 ) ) ;
#6116 = CARTESIAN_POINT ( 'NONE',  ( 0.000000000000000000, 0.000000000000000000, 1.000000000000000000 ) ) ;
#6117 = CARTESIAN_POINT ( 'NONE',  ( -9.296355089585909904E-15, 29.10624999877097352, 4.999999999999992006 ) ) ;
#6118 = CARTESIAN_POINT ( 'NONE',  ( -3.999999999999996447, -8.999999999999992895, 2.925000000000000711 ) ) ;
#6119 = ORIENTED_EDGE ( 'NONE', *, *, #3875, .F. ) ;
#6120 = CARTESIAN_POINT ( 'NONE',  ( 1.500000000000001776, -10.49999999999999289, 4.999999999999993783 ) ) ;
#6121 = CARTESIAN_POINT ( 'NONE',  ( -1.999999999999998224, 26.14374999877096784, 12.46410161513774639 ) ) ;
#6122 = CARTESIAN_POINT ( 'NONE',  ( 8.217531866531087914, 29.99470236596032535, 1.000000000000000000 ) ) ;
#6124 = ORIENTED_EDGE ( 'NONE', *, *, #2278, .T. ) ;
#6123 = DIRECTION ( 'NONE',  ( -0.000000000000000000, -0.000000000000000000, -1.000000000000000000 ) ) ;
#6125 = ORIENTED_EDGE ( 'NONE', *, *, #2638, .F. ) ;
#6126 = VERTEX_POINT ( 'NONE', #4101 ) ;
#6127 = EDGE_LOOP ( 'NONE', ( #16407, #643, #10816, #7298 ) ) ;
#6128 = ADVANCED_FACE ( 'NONE', ( #21771 ), #11832, .F. ) ;
#6129 = CARTESIAN_POINT ( 'NONE',  ( 21.28941499438209206, -22.67092431280601872, 1.000000000000000000 ) ) ;
#6130 = CARTESIAN_POINT ( 'NONE',  ( 1.878215178125008489, 26.22812499938548925, 5.746835883940462963 ) ) ;
#6131 =( LENGTH_UNIT ( ) NAMED_UNIT ( * ) SI_UNIT ( .MILLI., .METRE. ) );
#6132 = EDGE_CURVE ( 'NONE', #9673, #7360, #2144, .T. ) ;
#6133 = CARTESIAN_POINT ( 'NONE',  ( 1.878215178125003382, 26.11562499938548854, 5.746835883940462963 ) ) ;
#6134 = ADVANCED_FACE ( 'NONE', ( #835 ), #20585, .T. ) ;
#6135 = CARTESIAN_POINT ( 'NONE',  ( 3.756430356250002323, -11.16877607737301226, 4.153124999385482852 ) ) ;
#6136 = CARTESIAN_POINT ( 'NONE',  ( -3.999999999999996003, -6.690598923241487306, 3.281249998770966236 ) ) ;
#6137 =( LENGTH_UNIT ( ) NAMED_UNIT ( * ) SI_UNIT ( .MILLI., .METRE. ) );
#6138 = CARTESIAN_POINT ( 'NONE',  ( 2.672651547586948120E-15, 26.37812499938548427, 13.33755215474602984 ) ) ;
#6139 = LINE ( 'NONE', #13999, #19246 ) ;
#6140 = DIRECTION ( 'NONE',  ( 0.000000000000000000, -0.000000000000000000, 1.000000000000000000 ) ) ;
#6141 = CARTESIAN_POINT ( 'NONE',  ( -1.878215178124995832, 25.29062499938548569, 5.746835883940462963 ) ) ;
#6142 = CARTESIAN_POINT ( 'NONE',  ( 29.72853858738281829, 9.133673601486481886, 1.000000000000000000 ) ) ;
#6143 = CARTESIAN_POINT ( 'NONE',  ( -5.577813053751546416E-15, -25.73124999877097352, 12.99999999999999289 ) ) ;
#6144 = LINE ( 'NONE', #6408, #16812 ) ;
#6145 = CARTESIAN_POINT ( 'NONE',  ( 1.878215178124995832, -25.40312499938548640, 5.746835883940462963 ) ) ;
#6146 = CARTESIAN_POINT ( 'NONE',  ( 3.735045420075836212E-15, 28.96562499938548640, 4.662447845253954171 ) ) ;
#6147 = CARTESIAN_POINT ( 'NONE',  ( -3.999999999999996447, -8.999999999999992895, 2.925000000000000711 ) ) ;
#6148 = CARTESIAN_POINT ( 'NONE',  ( 3.756430356250003655, 25.19687499938548569, 8.999999999999992895 ) ) ;
#6149 = FACE_OUTER_BOUND ( 'NONE', #18414, .T. ) ;
#6150 = VERTEX_POINT ( 'NONE', #24246 ) ;
#6151 = CARTESIAN_POINT ( 'NONE',  ( -2.000000000000000888, -28.97500000000000142, 12.46410161513774817 ) ) ;
#6153 = ORIENTED_EDGE ( 'NONE', *, *, #17946, .F. ) ;
#6152 = CARTESIAN_POINT ( 'NONE',  ( 0.000000000000000000, 0.000000000000000000, -6.500000000000000000 ) ) ;
#6154 = ORIENTED_EDGE ( 'NONE', *, *, #16272, .F. ) ;
#6155 = VERTEX_POINT ( 'NONE', #8292 ) ;
#6156 = VERTEX_POINT ( 'NONE', #22409 ) ;
#6157 = ORIENTED_EDGE ( 'NONE', *, *, #17323, .T. ) ;
#6158 = LINE ( 'NONE', #17815, #6300 ) ;
#6159 = EDGE_LOOP ( 'NONE', ( #9156, #3979 ) ) ;
#6160 = EDGE_CURVE ( 'NONE', #380, #2254, #22546, .T. ) ;
#6161 = CARTESIAN_POINT ( 'NONE',  ( 3.469446951953614189E-15, 39.50000000000000000, 8.999999999999992895 ) ) ;
#6162 = CARTESIAN_POINT ( 'NONE',  ( 2.672651547586948120E-15, 25.59062499938548640, 13.33755215474603162 ) ) ;
#6163 = EDGE_CURVE ( 'NONE', #11292, #523, #24385, .T. ) ;
#6164 = CARTESIAN_POINT ( 'NONE',  ( 1.878215178125004048, -5.746835883940462963, 2.578124999385485339 ) ) ;
#6165 = CARTESIAN_POINT ( 'NONE',  ( 3.469446951953614189E-15, 39.50000000000000000, 8.999999999999992895 ) ) ;
#6166 = CARTESIAN_POINT ( 'NONE',  ( 18.14606400620158411, 20.80226138416088588, 5.746835883940462963 ) ) ;
#6167 = EDGE_CURVE ( 'NONE', #20633, #6625, #462, .T. ) ;
#6168 = CARTESIAN_POINT ( 'NONE',  ( 20.46190248058575634, 20.46190248058568173, 12.99999999999999289 ) ) ;
#6169 = FILL_AREA_STYLE_COLOUR ( '', #16308 ) ;
#6170 = VECTOR ( 'NONE', #25169, 1000.000000000000000 ) ;
#6171 = CARTESIAN_POINT ( 'NONE',  ( -3.756430356249996994, -8.999999999999992895, 1.715624999385483074 ) ) ;
#6172 = CARTESIAN_POINT ( 'NONE',  ( 4.000000000000003553, 27.73750000000000071, 6.690598923241489970 ) ) ;
#6173 = CARTESIAN_POINT ( 'NONE',  ( 2.000000000000003997, 29.12500000000000000, 5.535898384862238508 ) ) ;
#6174 = CARTESIAN_POINT ( 'NONE',  ( 3.999999999999987121, -11.30940107675850648, 3.562499999999996891 ) ) ;
#6175 = CARTESIAN_POINT ( 'NONE',  ( -0.7500000000000000000, -2.999999999999999556, 17.69999999999999929 ) ) ;
#6176 = CARTESIAN_POINT ( 'NONE',  ( 8.831537335106614961E-15, 27.53124999877097068, 12.99999999999999112 ) ) ;
#6177 = ORIENTED_EDGE ( 'NONE', *, *, #3638, .F. ) ;
#6178 = ORIENTED_EDGE ( 'NONE', *, *, #22992, .T. ) ;
#6179 = CARTESIAN_POINT ( 'NONE',  ( 4.006172263299091013E-15, 25.36562499938549564, 4.662447845253954171 ) ) ;
#6180 = ORIENTED_EDGE ( 'NONE', *, *, #21709, .T. ) ;
#6181 = CARTESIAN_POINT ( 'NONE',  ( -22.32573188046936252, -21.65113613650319380, -2.750000000000000000 ) ) ;
#6182 = CARTESIAN_POINT ( 'NONE',  ( 3.752267015613588906E-15, 29.55624999877096926, 4.381197846482986158 ) ) ;
#6183 = CARTESIAN_POINT ( 'NONE',  ( -1.878215178124998497, 29.15312499938548640, 12.25316411605951927 ) ) ;
#6184 = CARTESIAN_POINT ( 'NONE',  ( 8.831537335106614961E-15, 27.53124999877097068, 12.99999999999999112 ) ) ;
#6185 = VERTEX_POINT ( 'NONE', #10241 ) ;
#6186 = CIRCLE ( 'NONE', #9534, 0.5000000000000004441 ) ;
#6187 = DIRECTION ( 'NONE',  ( 1.000000000000000000, 0.000000000000000000, 0.000000000000000000 ) ) ;
#6188 = EDGE_LOOP ( 'NONE', ( #20771, #24778, #18707, #24693 ) ) ;
#6189 = DIRECTION ( 'NONE',  ( 0.000000000000000000, 0.000000000000000000, 1.000000000000000000 ) ) ;
#6190 = EDGE_CURVE ( 'NONE', #4202, #2078, #2791, .T. ) ;
#6191 = CARTESIAN_POINT ( 'NONE',  ( -1.878215178124998497, 27.69062499938548427, 12.25316411605951927 ) ) ;
#6192 = EDGE_CURVE ( 'NONE', #485, #672, #23845, .T. ) ;
#6193 = AXIS2_PLACEMENT_3D ( 'NONE', #13229, #3278, #19232 ) ;
#6194 = CARTESIAN_POINT ( 'NONE',  ( 0.2821657309629718169, 38.91194779626418665, 3.418731683527081344 ) ) ;
#6195 = CARTESIAN_POINT ( 'NONE',  ( 3.469446951953614189E-15, 35.50000000000000711, 8.999999999999992895 ) ) ;
#6196 = CARTESIAN_POINT ( 'NONE',  ( 3.063240906311874401, 29.84319947910909931, 11.57226653943513028 ) ) ;
#6197 = CARTESIAN_POINT ( 'NONE',  ( -1.878215178124998497, 26.79062499938548214, 12.25316411605951927 ) ) ;
#6198 = EDGE_CURVE ( 'NONE', #1528, #14319, #20521, .T. ) ;
#6199 = CARTESIAN_POINT ( 'NONE',  ( 4.000000000000003553, -8.999999999999992895, 1.293749998770969079 ) ) ;
#6200 = AXIS2_PLACEMENT_3D ( 'NONE', #15039, #20925, #18963 ) ;
#6201 = AXIS2_PLACEMENT_3D ( 'NONE', #15550, #11739, #7693 ) ;
#6202 = CARTESIAN_POINT ( 'NONE',  ( -1.999999999999998224, -12.46410161513774639, 2.100000000000000977 ) ) ;
#6203 = DIRECTION ( 'NONE',  ( 0.000000000000000000, 0.000000000000000000, 1.000000000000000000 ) ) ;
#6204 = CARTESIAN_POINT ( 'NONE',  ( -3.918924903856942255, -29.74337361029841276, 9.928636277907717300 ) ) ;
#6205 = DIRECTION ( 'NONE',  ( 0.000000000000000000, 0.000000000000000000, 1.000000000000000000 ) ) ;
#6207 = CARTESIAN_POINT ( 'NONE',  ( -1.071796769724487230, 25.13259618943233420, 4.999999999999992006 ) ) ;
#6206 = AXIS2_PLACEMENT_3D ( 'NONE', #3324, #21002, #9084 ) ;
#6208 = CARTESIAN_POINT ( 'NONE',  ( -3.959305671612554781E-15, -30.00000000000000355, 12.99999999999999289 ) ) ;
#6209 = AXIS2_PLACEMENT_3D ( 'NONE', #18, #21857, #16223 ) ;
#6210 = VERTEX_POINT ( 'NONE', #12345 ) ;
#6211 = CARTESIAN_POINT ( 'NONE',  ( -1.999999999999998224, 28.84374999877096712, 12.46410161513774639 ) ) ;
#6212 = CARTESIAN_POINT ( 'NONE',  ( -4.000000000000003553, -29.50000000000000355, 8.999999999999992895 ) ) ;
#6214 = EDGE_LOOP ( 'NONE', ( #8723, #15432, #22137, #10428 ) ) ;
#6213 = CARTESIAN_POINT ( 'NONE',  ( -3.756430356249996549, 27.69062499938548072, 6.831223922626973533 ) ) ;
#6215 = CARTESIAN_POINT ( 'NONE',  ( 3.756430356250003655, 27.95312499938548711, 8.999999999999992895 ) ) ;
#6216 = CARTESIAN_POINT ( 'NONE',  ( 1.071796769724494114, 27.15759618943233988, 12.99999999999999112 ) ) ;
#6217 = CARTESIAN_POINT ( 'NONE',  ( 3.369928719974892281E-15, 25.50624999877096855, 4.999999999999992006 ) ) ;
#6218 = ORIENTED_EDGE ( 'NONE', *, *, #3370, .T. ) ;
#6219 = ORIENTED_EDGE ( 'NONE', *, *, #390, .T. ) ;
#6220 = CARTESIAN_POINT ( 'NONE',  ( -3.756430356250003211, -27.54062499938547859, 6.831223922626973533 ) ) ;
#6221 = CARTESIAN_POINT ( 'NONE',  ( -1.878215178124996498, 28.44062499938548783, 5.746835883940462963 ) ) ;
#6222 = CARTESIAN_POINT ( 'NONE',  ( -2.000000000000003997, -29.06874999877096855, 5.535898384862238508 ) ) ;
#6223 = VECTOR ( 'NONE', #16290, 1000.000000000000000 ) ;
#6224 = CARTESIAN_POINT ( 'NONE',  ( 3.756430356250003211, -6.831223922626973533, 2.878124999385481608 ) ) ;
#6225 = AXIS2_PLACEMENT_3D ( 'NONE', #9454, #7488, #15477 ) ;
#6226 = VECTOR ( 'NONE', #4840, 1000.000000000000000 ) ;
#6227 = EDGE_CURVE ( 'NONE', #3169, #19826, #23036, .T. ) ;
#6228 = CARTESIAN_POINT ( 'NONE',  ( -27.10000000000000497, -0.5999999999999998668, 19.59999999999999787 ) ) ;
#6229 = SURFACE_SIDE_STYLE ('',( #18022 ) ) ;
#6230 =( BOUNDED_CURVE ( )  B_SPLINE_CURVE ( 2, ( #22010, #21502, #11682, #17967, #7764, #23463, #12063, #19519, #3842 ),
 .UNSPECIFIED., .F., .F. ) 
 B_SPLINE_CURVE_WITH_KNOTS ( ( 3, 2, 2, 2, 3 ),
 ( 0.2750000000000000222, 0.2833333333333333259, 0.2999999999999999889, 0.3166666666666666519, 0.3250000000000000111 ),
 .UNSPECIFIED. ) 
 CURVE ( )  GEOMETRIC_REPRESENTATION_ITEM ( )  RATIONAL_B_SPLINE_CURVE ( ( 0.9330127018922194093, 0.9330127018922196314, 1.000000000000000000, 0.8660254037844387076, 1.000000000000000000, 0.8660254037844387076, 1.000000000000000000, 0.9330127018922191873, 0.9330127018922194093 ) ) 
 REPRESENTATION_ITEM ( '' )  );
#6231 =( BOUNDED_CURVE ( )  B_SPLINE_CURVE ( 2, ( #8974, #1110, #17071, #25043, #24917, #7133, #24520, #16949, #21119 ),
 .UNSPECIFIED., .F., .F. ) 
 B_SPLINE_CURVE_WITH_KNOTS ( ( 3, 2, 2, 2, 3 ),
 ( 0.1749999999999999889, 0.1833333333333333204, 0.2000000000000000111, 0.2166666666666666741, 0.2250000000000000056 ),
 .UNSPECIFIED. ) 
 CURVE ( )  GEOMETRIC_REPRESENTATION_ITEM ( )  RATIONAL_B_SPLINE_CURVE ( ( 0.9330127018922194093, 0.9330127018922194093, 1.000000000000000000, 0.8660254037844387076, 1.000000000000000000, 0.8660254037844387076, 1.000000000000000000, 0.9330127018922194093, 0.9330127018922194093 ) ) 
 REPRESENTATION_ITEM ( '' )  );
#6232 = DIRECTION ( 'NONE',  ( -0.000000000000000000, 0.000000000000000000, 1.000000000000000000 ) ) ;
#6233 = DIRECTION ( 'NONE',  ( 0.000000000000000000, -1.000000000000000000, 0.000000000000000000 ) ) ;
#6234 = CARTESIAN_POINT ( 'NONE',  ( 3.469446951953614189E-15, -8.999999999999992895, 18.00000000000000000 ) ) ;
#6235 = AXIS2_PLACEMENT_3D ( 'NONE', #11909, #21724, #3809 ) ;
#6236 = CARTESIAN_POINT ( 'NONE',  ( 18.19474136253732865, 18.19474136253726826, 12.99999999999999289 ) ) ;
#6237 = CARTESIAN_POINT ( 'NONE',  ( -16.66421332384701515, -26.25859848311253941, -6.500000000000000000 ) ) ;
#6238 = CARTESIAN_POINT ( 'NONE',  ( 22.05081056025715114, 16.73841580433833442, 6.831223922626973533 ) ) ;
#6239 = CARTESIAN_POINT ( 'NONE',  ( 18.02680350200553150, 20.85523062675164851, 12.46410161513774639 ) ) ;
#6240 = EDGE_LOOP ( 'NONE', ( #4576, #25529, #4006, #18144 ) ) ;
#6241 = DIRECTION ( 'NONE',  ( 0.000000000000000000, 0.000000000000000000, 1.000000000000000000 ) ) ;
#6242 = CYLINDRICAL_SURFACE ( 'NONE', #9237, 0.5000000000000004441 ) ;
#6243 =( BOUNDED_CURVE ( )  B_SPLINE_CURVE ( 2, ( #20748, #12901, #2827, #20344, #8857, #4669, #499, #24807, #2440 ),
 .UNSPECIFIED., .F., .F. ) 
 B_SPLINE_CURVE_WITH_KNOTS ( ( 3, 2, 2, 2, 3 ),
 ( 0.4250000000000000444, 0.4333333333333333481, 0.4500000000000000111, 0.4666666666666666741, 0.4750000000000000333 ),
 .UNSPECIFIED. ) 
 CURVE ( )  GEOMETRIC_REPRESENTATION_ITEM ( )  RATIONAL_B_SPLINE_CURVE ( ( 0.9330127018922194093, 0.9330127018922196314, 1.000000000000000000, 0.8660254037844387076, 1.000000000000000000, 0.8660254037844387076, 1.000000000000000000, 0.9330127018922191873, 0.9330127018922194093 ) ) 
 REPRESENTATION_ITEM ( '' )  );
#6244 = CARTESIAN_POINT ( 'NONE',  ( 1.878215178125000939, 25.51562499938548356, 12.25316411605952283 ) ) ;
#6246 = ORIENTED_EDGE ( 'NONE', *, *, #1611, .F. ) ;
#6245 = CARTESIAN_POINT ( 'NONE',  ( -3.796077574538131660, 29.75903253174124430, 10.28786097927510923 ) ) ;
#6247 = AXIS2_PLACEMENT_3D ( 'NONE', #13210, #23025, #11369 ) ;
#6248 = CYLINDRICAL_SURFACE ( 'NONE', #13340, 4.000000000000000000 ) ;
#6249 = DIRECTION ( 'NONE',  ( 0.000000000000000000, 1.000000000000000000, 0.000000000000000000 ) ) ;
#6250 = ORIENTED_EDGE ( 'NONE', *, *, #20484, .T. ) ;
#6251 = CARTESIAN_POINT ( 'NONE',  ( -27.10000000000000497, 0.6000000000000000888, 19.59999999999999787 ) ) ;
#6252 = DIRECTION ( 'NONE',  ( 0.000000000000000000, -0.000000000000000000, 1.000000000000000000 ) ) ;
#6253 = CARTESIAN_POINT ( 'NONE',  ( 1.878215178124998497, -27.24062499938548498, 12.25316411605951927 ) ) ;
#6255 = ORIENTED_EDGE ( 'NONE', *, *, #21074, .T. ) ;
#6254 = DIRECTION ( 'NONE',  ( 1.000000000000000000, 0.000000000000000000, 0.000000000000000000 ) ) ;
#6256 = AXIS2_PLACEMENT_3D ( 'NONE', #22513, #6682, #14672 ) ;
#6258 = ORIENTED_EDGE ( 'NONE', *, *, #10353, .T. ) ;
#6257 = CIRCLE ( 'NONE', #23782, 31.10000000000000142 ) ;
#6259 = ORIENTED_EDGE ( 'NONE', *, *, #5664, .T. ) ;
#6260 = VERTEX_POINT ( 'NONE', #14566 ) ;
#6261 = LINE ( 'NONE', #7713, #14730 ) ;
#6262 = CARTESIAN_POINT ( 'NONE',  ( 3.756430356250004543, 25.29062499938548925, 6.831223922626973533 ) ) ;
#6263 = AXIS2_PLACEMENT_3D ( 'NONE', #15686, #24041, #11754 ) ;
#6264 = CARTESIAN_POINT ( 'NONE',  ( -3.999999999999996447, 26.51874999877097139, 8.999999999999992895 ) ) ;
#6265 = EDGE_CURVE ( 'NONE', #16682, #4650, #16208, .T. ) ;
#6266 = CARTESIAN_POINT ( 'NONE',  ( -3.999999999999996447, 28.82500000000000284, 8.999999999999992895 ) ) ;
#6267 = CARTESIAN_POINT ( 'NONE',  ( -3.999999999999996447, -8.999999999999992895, 4.218749998770966236 ) ) ;
#6268 =( NAMED_UNIT ( * ) PLANE_ANGLE_UNIT ( ) SI_UNIT ( $, .RADIAN. ) );
#6269 = CARTESIAN_POINT ( 'NONE',  ( 2.672651547586948120E-15, 26.82812499938548356, 13.33755215474602984 ) ) ;
#6270 = VECTOR ( 'NONE', #20027, 1000.000000000000000 ) ;
#6271 = ADVANCED_FACE ( 'NONE', ( #2403 ), #24627, .T. ) ;
#6272 = DIRECTION ( 'NONE',  ( 0.000000000000000000, 0.000000000000000000, 1.000000000000000000 ) ) ;
#6273 = CARTESIAN_POINT ( 'NONE',  ( 3.469446951953614189E-15, 35.50000000000000711, 8.999999999999992895 ) ) ;
#6274 = CARTESIAN_POINT ( 'NONE',  ( 2.672651547586948120E-15, 27.27812499938548640, 13.33755215474603162 ) ) ;
#6275 = LINE ( 'NONE', #14266, #15480 ) ;
#6276 = CARTESIAN_POINT ( 'NONE',  ( 1.071796769724495446, 26.38615380933864074, 4.999999999999992895 ) ) ;
#6277 = CARTESIAN_POINT ( 'NONE',  ( 20.92219106202043122, -23.01025686871645348, 1.000000000000000000 ) ) ;
#6278 = EDGE_CURVE ( 'NONE', #4122, #15349, #18747, .T. ) ;
#6279 = CARTESIAN_POINT ( 'NONE',  ( 1.878215178124998497, -25.55312499938548854, 12.25316411605951927 ) ) ;
#6280 = CARTESIAN_POINT ( 'NONE',  ( 3.469446951953614189E-15, -8.999999999999992895, 18.00000000000000000 ) ) ;
#6281 = DIRECTION ( 'NONE',  ( -0.7071067811865487940, -0.7071067811865463515, 0.000000000000000000 ) ) ;
#6282 = AXIS2_PLACEMENT_3D ( 'NONE', #60, #24236, #6322 ) ;
#6283 = CARTESIAN_POINT ( 'NONE',  ( -20.92219106202016476, 23.01025686871669507, -2.750000000000000000 ) ) ;
#6284 = DIRECTION ( 'NONE',  ( 0.000000000000000000, 0.000000000000000000, 1.000000000000000000 ) ) ;
#6285 = EDGE_LOOP ( 'NONE', ( #13987, #9602, #2460, #15231 ) ) ;
#6286 = ADVANCED_FACE ( 'NONE', ( #22156 ), #4490, .T. ) ;
#6287 = LINE ( 'NONE', #4844, #22545 ) ;
#6289 = ORIENTED_EDGE ( 'NONE', *, *, #22830, .T. ) ;
#6288 = CYLINDRICAL_SURFACE ( 'NONE', #7482, 0.5000000000000004441 ) ;
#6290 = CIRCLE ( 'NONE', #21743, 0.5000000000000006661 ) ;
#6291 = VECTOR ( 'NONE', #6769, 1000.000000000000000 ) ;
#6292 = ORIENTED_EDGE ( 'NONE', *, *, #21461, .T. ) ;
#6293 = ORIENTED_EDGE ( 'NONE', *, *, #20736, .T. ) ;
#6294 = VERTEX_POINT ( 'NONE', #2286 ) ;
#6295 = ORIENTED_EDGE ( 'NONE', *, *, #16004, .F. ) ;
#6296 = CARTESIAN_POINT ( 'NONE',  ( 0.000000000000000000, 0.000000000000000000, -6.500000000000000000 ) ) ;
#6297 = AXIS2_PLACEMENT_3D ( 'NONE', #19954, #4281, #2060 ) ;
#6298 = ORIENTED_EDGE ( 'NONE', *, *, #21496, .F. ) ;
#6299 = CARTESIAN_POINT ( 'NONE',  ( -3.756430356249997438, 25.96562499938548640, 11.16877607737301048 ) ) ;
#6300 = VECTOR ( 'NONE', #9953, 1000.000000000000000 ) ;
#6301 = CARTESIAN_POINT ( 'NONE',  ( -1.878215178124995832, -5.746835883940462963, 1.753124999385485827 ) ) ;
#6302 = CARTESIAN_POINT ( 'NONE',  ( 3.999999999999954259, -6.690598923241460660, 1.331249998770968057 ) ) ;
#6303 = CARTESIAN_POINT ( 'NONE',  ( 20.32496430686003208, 17.66876692890059530, 12.25316411605952283 ) ) ;
#6304 = AXIS2_PLACEMENT_3D ( 'NONE', #17385, #15418, #23647 ) ;
#6305 = FACE_OUTER_BOUND ( 'NONE', #17058, .T. ) ;
#6306 = VECTOR ( 'NONE', #4744, 1000.000000000000000 ) ;
#6307 = CARTESIAN_POINT ( 'NONE',  ( 1.878215178125000939, -12.25316411605952283, 1.415624999385481253 ) ) ;
#6308 = DIRECTION ( 'NONE',  ( 0.000000000000000000, 0.000000000000000000, 1.000000000000000000 ) ) ;
#6309 = CARTESIAN_POINT ( 'NONE',  ( 3.756430356250003211, 28.32812499938548356, 6.831223922626973533 ) ) ;
#6310 = AXIS2_PLACEMENT_3D ( 'NONE', #3208, #7394, #3598 ) ;
#6311 = CARTESIAN_POINT ( 'NONE',  ( 3.735045420075836212E-15, -4.662447845253954171, 1.715624999385482852 ) ) ;
#6312 = CARTESIAN_POINT ( 'NONE',  ( -1.999999999999995781, 27.40000000000000213, 5.535898384862237620 ) ) ;
#6313 = ORIENTED_EDGE ( 'NONE', *, *, #1804, .F. ) ;
#6314 = EDGE_CURVE ( 'NONE', #3260, #19788, #55, .T. ) ;
#6315 = EDGE_LOOP ( 'NONE', ( #21342, #20459, #15848, #8384 ) ) ;
#6316 = CARTESIAN_POINT ( 'NONE',  ( -3.756430356249996549, 27.27812499938548996, 8.999999999999992895 ) ) ;
#6317 = EDGE_CURVE ( 'NONE', #9218, #20930, #6723, .T. ) ;
#6318 = CIRCLE ( 'NONE', #11313, 0.5000000000000003331 ) ;
#6319 = ORIENTED_EDGE ( 'NONE', *, *, #1907, .F. ) ;
#6320 = CARTESIAN_POINT ( 'NONE',  ( 2.000000000000003997, 25.07499999999999929, 5.535898384862238508 ) ) ;
#6321 = EDGE_LOOP ( 'NONE', ( #21146, #4388, #14760, #11756 ) ) ;
#6322 = DIRECTION ( 'NONE',  ( -0.9510565162951518658, 0.3090169943749528914, 0.000000000000000000 ) ) ;
#6323 = ORIENTED_EDGE ( 'NONE', *, *, #18309, .F. ) ;
#6324 = EDGE_CURVE ( 'NONE', #14520, #18733, #18892, .T. ) ;
#6325 = AXIS2_PLACEMENT_3D ( 'NONE', #13043, #3100, #11959 ) ;
#6326 = AXIS2_PLACEMENT_3D ( 'NONE', #9654, #15410, #9274 ) ;
#6327 = FACE_OUTER_BOUND ( 'NONE', #7928, .T. ) ;
#6328 = EDGE_LOOP ( 'NONE', ( #11439, #24472, #8731, #17251, #10496, #4062, #7475, #8449, #21067, #17501, #1761, #2449, #1439, #17143, #62, #751 ) ) ;
#6329 = CARTESIAN_POINT ( 'NONE',  ( -3.469446951953614189E-15, -30.00000000000000355, 8.999999999999992895 ) ) ;
#6330 = CARTESIAN_POINT ( 'NONE',  ( 3.735045420075836212E-15, 27.50312499938548783, 4.662447845253954171 ) ) ;
#6331 = DIRECTION ( 'NONE',  ( 0.000000000000000000, -0.000000000000000000, 1.000000000000000000 ) ) ;
#6332 = AXIS2_PLACEMENT_3D ( 'NONE', #9404, #5474, #17266 ) ;
#6333 = DIRECTION ( 'NONE',  ( 0.000000000000000000, 0.000000000000000000, 1.000000000000000000 ) ) ;
#6334 = CARTESIAN_POINT ( 'NONE',  ( -24.27856662945480792, 19.43607991389014344, -6.500000000000000000 ) ) ;
#6335 = CARTESIAN_POINT ( 'NONE',  ( 3.677829432474411853, 29.77381621822422275, 10.59017455026297405 ) ) ;
#6336 = AXIS2_PLACEMENT_3D ( 'NONE', #7926, #19941, #451 ) ;
#6337 = CARTESIAN_POINT ( 'NONE',  ( 2.672651547586948120E-15, 28.62812499938548783, 13.33755215474602984 ) ) ;
#6338 = DIRECTION ( 'NONE',  ( -1.000000000000000000, 0.000000000000000000, -0.000000000000000000 ) ) ;
#6339 = EDGE_CURVE ( 'NONE', #18733, #14017, #18942, .T. ) ;
#6340 = CARTESIAN_POINT ( 'NONE',  ( 19.02117241391816904, 21.84959953866428606, 12.46410161513774639 ) ) ;
#6341 = CARTESIAN_POINT ( 'NONE',  ( -1.999999999999995781, 29.19999999999999929, 5.535898384862237620 ) ) ;
#6342 = CARTESIAN_POINT ( 'NONE',  ( 1.071796769724481901, -27.96115380933863293, 12.99999999999999645 ) ) ;
#6343 = VECTOR ( 'NONE', #15678, 1000.000000000000000 ) ;
#6345 = EDGE_CURVE ( 'NONE', #16937, #23824, #1741, .T. ) ;
#6344 = CARTESIAN_POINT ( 'NONE',  ( -1.071796769724487230, 25.31740381056767220, 12.99999999999999467 ) ) ;
#6346 = CARTESIAN_POINT ( 'NONE',  ( -1.999999999999995781, -5.535898384862237620, 1.500000000000001332 ) ) ;
#6347 = ORIENTED_EDGE ( 'NONE', *, *, #6574, .F. ) ;
#6348 = CARTESIAN_POINT ( 'NONE',  ( 4.000000000000003553, 26.74374999877096926, 8.999999999999992895 ) ) ;
#6349 = CARTESIAN_POINT ( 'NONE',  ( 3.999999999999996003, -27.88750000000000284, 6.690598923241487306 ) ) ;
#6351 = ORIENTED_EDGE ( 'NONE', *, *, #9460, .F. ) ;
#6350 = CARTESIAN_POINT ( 'NONE',  ( 3.756430356250001434, 27.50312499938548783, 8.999999999999992895 ) ) ;
#6352 = ORIENTED_EDGE ( 'NONE', *, *, #22188, .T. ) ;
#6353 = CARTESIAN_POINT ( 'NONE',  ( -1.999999999999995781, 28.69374999877096855, 5.535898384862237620 ) ) ;
#6354 = AXIS2_PLACEMENT_3D ( 'NONE', #3817, #15849, #20275 ) ;
#6355 =( BOUNDED_CURVE ( )  B_SPLINE_CURVE ( 2, ( #8441, #14337, #2032, #14579, #22558, #19929, #18372, #6342, #18247 ),
 .UNSPECIFIED., .F., .F. ) 
 B_SPLINE_CURVE_WITH_KNOTS ( ( 3, 2, 2, 2, 3 ),
 ( 0.5250000000000000222, 0.5333333333333333259, 0.5500000000000000444, 0.5666666666666666519, 0.5750000000000000666 ),
 .UNSPECIFIED. ) 
 CURVE ( )  GEOMETRIC_REPRESENTATION_ITEM ( )  RATIONAL_B_SPLINE_CURVE ( ( 0.9330127018922194093, 0.9330127018922194093, 1.000000000000000000, 0.8660254037844387076, 1.000000000000000000, 0.8660254037844387076, 1.000000000000000000, 0.9330127018922189652, 0.9330127018922194093 ) ) 
 REPRESENTATION_ITEM ( '' )  );
#6356 = CYLINDRICAL_SURFACE ( 'NONE', #23835, 31.10000000000000142 ) ;
#6357 = CARTESIAN_POINT ( 'NONE',  ( -1.999999999999995781, 27.79374999877096997, 5.535898384862237620 ) ) ;
#6358 = ORIENTED_EDGE ( 'NONE', *, *, #9183, .F. ) ;
#6359 = ORIENTED_EDGE ( 'NONE', *, *, #3657, .F. ) ;
#6360 = CARTESIAN_POINT ( 'NONE',  ( 1.878215178124998497, -27.35312499938548569, 12.25316411605951927 ) ) ;
#6361 = AXIS2_PLACEMENT_3D ( 'NONE', #3627, #25470, #19330 ) ;
#6362 = CARTESIAN_POINT ( 'NONE',  ( 1.878215178124998275, 26.86562499938548854, 12.25316411605952283 ) ) ;
#6363 = CARTESIAN_POINT ( 'NONE',  ( -30.12293631110035363, 7.734255490827311341, 1.000000000000000000 ) ) ;
#6364 = AXIS2_PLACEMENT_3D ( 'NONE', #15034, #23014, #3131 ) ;
#6365 = ADVANCED_FACE ( 'NONE', ( #6976 ), #22932, .F. ) ;
#6366 = CARTESIAN_POINT ( 'NONE',  ( 29.57785765677931167, 9.610428525060783045, 1.000000000000000000 ) ) ;
#6367 = CARTESIAN_POINT ( 'NONE',  ( -4.000000000000033751, -6.690598923241509510, 1.087499999999997025 ) ) ;
#6368 = SURFACE_STYLE_FILL_AREA ( #11979 ) ;
#6369 = DIRECTION ( 'NONE',  ( 0.000000000000000000, 0.000000000000000000, -1.000000000000000000 ) ) ;
#6370 = CARTESIAN_POINT ( 'NONE',  ( -3.999999999999996447, -8.999999999999992895, 3.374999999999999556 ) ) ;
#6371 = VECTOR ( 'NONE', #23750, 1000.000000000000000 ) ;
#6372 = CARTESIAN_POINT ( 'NONE',  ( 3.469446951953614189E-15, -8.999999999999992895, 8.000000000000000000 ) ) ;
#6373 = CARTESIAN_POINT ( 'NONE',  ( 5.577813053751546416E-15, 25.33750000000000213, 12.99999999999999289 ) ) ;
#6374 = CARTESIAN_POINT ( 'NONE',  ( 15.91640417120904871, 21.22879892712773042, 8.999999999999992895 ) ) ;
#6375 = CARTESIAN_POINT ( 'NONE',  ( 18.55713358789543932, 21.38556071264155634, 5.535898384862237620 ) ) ;
#6376 = ORIENTED_EDGE ( 'NONE', *, *, #17793, .F. ) ;
#6377 = CARTESIAN_POINT ( 'NONE',  ( -5.432449689414484695, 38.61000136877622424, 11.27614500780635431 ) ) ;
#6378 = CARTESIAN_POINT ( 'NONE',  ( 3.469446951953614189E-15, 30.00000000000000355, 4.999999999999992006 ) ) ;
#6379 = CARTESIAN_POINT ( 'NONE',  ( 1.878215178125000939, 25.96562499938548285, 12.25316411605952283 ) ) ;
#6380 = AXIS2_PLACEMENT_3D ( 'NONE', #4868, #2776, #816 ) ;
#6382 = VERTEX_POINT ( 'NONE', #15341 ) ;
#6381 = CARTESIAN_POINT ( 'NONE',  ( -2.642157743709451889, 29.88401080970086099, 12.01472878375391140 ) ) ;
#6383 = CARTESIAN_POINT ( 'NONE',  ( 20.43330379829292198, 15.12090904237410527, 8.999999999999992895 ) ) ;
#6384 = CARTESIAN_POINT ( 'NONE',  ( 20.20656826142266738, -23.64116323484245541, 1.000000000000000000 ) ) ;
#6385 = VERTEX_POINT ( 'NONE', #13385 ) ;
#6386 = CYLINDRICAL_SURFACE ( 'NONE', #23444, 0.7500000000000001110 ) ;
#6387 = CARTESIAN_POINT ( 'NONE',  ( 4.000000000000001776, 26.70624999877097139, 11.30940107675849760 ) ) ;
#6388 = CARTESIAN_POINT ( 'NONE',  ( -3.735045420075836212E-15, -25.70312499938548001, 4.662447845253954171 ) ) ;
#6390 = ORIENTED_EDGE ( 'NONE', *, *, #5142, .T. ) ;
#6389 = DIRECTION ( 'NONE',  ( 1.000000000000000000, 0.000000000000000000, 0.000000000000000000 ) ) ;
#6391 = ADVANCED_FACE ( 'NONE', ( #13250 ), #3303, .F. ) ;
#6392 = AXIS2_PLACEMENT_3D ( 'NONE', #10885, #11027, #6711 ) ;
#6393 = VERTEX_POINT ( 'NONE', #11028 ) ;
#6394 = CARTESIAN_POINT ( 'NONE',  ( 3.756430356249997882, -25.40312499938548285, 11.16877607737301226 ) ) ;
#6395 = EDGE_LOOP ( 'NONE', ( #21419, #17397, #20143, #22060 ) ) ;
#6396 = ORIENTED_EDGE ( 'NONE', *, *, #15366, .T. ) ;
#6397 = CARTESIAN_POINT ( 'NONE',  ( -2.003086131649545506E-15, 26.49062499938548143, 13.33755215474602984 ) ) ;
#6398 = CARTESIAN_POINT ( 'NONE',  ( 3.735045420075836212E-15, -4.662447845253954171, 4.303124999385482319 ) ) ;
#6399 = CARTESIAN_POINT ( 'NONE',  ( -3.756430356249995661, -6.831223922626973533, 3.140624999385484006 ) ) ;
#6400 =( BOUNDED_CURVE ( )  B_SPLINE_CURVE ( 2, ( #23183, #3294, #13378, #3436, #19383, #1477, #9449, #17558, #25533 ),
 .UNSPECIFIED., .F., .F. ) 
 B_SPLINE_CURVE_WITH_KNOTS ( ( 3, 2, 2, 2, 3 ),
 ( 0.3750000000000000000, 0.3833333333333333592, 0.4000000000000000222, 0.4166666666666666852, 0.4250000000000000444 ),
 .UNSPECIFIED. ) 
 CURVE ( )  GEOMETRIC_REPRESENTATION_ITEM ( )  RATIONAL_B_SPLINE_CURVE ( ( 0.9330127018922194093, 0.9330127018922194093, 1.000000000000000000, 0.8660254037844387076, 1.000000000000000000, 0.8660254037844387076, 1.000000000000000000, 0.9330127018922191873, 0.9330127018922194093 ) ) 
 REPRESENTATION_ITEM ( '' )  );
#6401 = CARTESIAN_POINT ( 'NONE',  ( 1.878215178125004048, 26.56562499938548427, 5.746835883940462963 ) ) ;
#6402 = CARTESIAN_POINT ( 'NONE',  ( -3.999999999999996447, -8.999999999999992895, 6.000000000000000000 ) ) ;
#6403 = CARTESIAN_POINT ( 'NONE',  ( 4.000000000000051514, -11.30940107675846917, 0.8624999999999993783 ) ) ;
#6404 = AXIS2_PLACEMENT_3D ( 'NONE', #21077, #4858, #23164 ) ;
#6405 = CARTESIAN_POINT ( 'NONE',  ( 2.672651547586948120E-15, 25.92812499938548498, 13.33755215474603162 ) ) ;
#6406 = CARTESIAN_POINT ( 'NONE',  ( 21.21320343559646915, 21.21320343559638744, 8.999999999999992895 ) ) ;
#6407 = DIRECTION ( 'NONE',  ( 1.000000000000000000, 0.000000000000000000, 0.000000000000000000 ) ) ;
#6408 = CARTESIAN_POINT ( 'NONE',  ( -3.999999999999996447, -8.999999999999992895, 18.00000000000000000 ) ) ;
#6409 = CARTESIAN_POINT ( 'NONE',  ( -4.000000000000003553, -28.09374999877097068, 8.999999999999992895 ) ) ;
#6410 = CARTESIAN_POINT ( 'NONE',  ( 4.000000000000003553, -8.999999999999992895, 2.193749998770967213 ) ) ;
#6411 = DIRECTION ( 'NONE',  ( 1.000000000000000000, 0.000000000000000000, 0.000000000000000000 ) ) ;
#6412 = VECTOR ( 'NONE', #2466, 1000.000000000000000 ) ;
#6413 = FACE_OUTER_BOUND ( 'NONE', #24072, .T. ) ;
#6414 = FACE_OUTER_BOUND ( 'NONE', #22402, .T. ) ;
#6415 = ORIENTED_EDGE ( 'NONE', *, *, #22425, .T. ) ;
#6416 = DIRECTION ( 'NONE',  ( 0.000000000000000000, -0.000000000000000000, 1.000000000000000000 ) ) ;
#6418 = EDGE_LOOP ( 'NONE', ( #2715, #9504, #23976, #12853 ) ) ;
#6417 = CYLINDRICAL_SURFACE ( 'NONE', #11657, 4.000000000000000000 ) ;
#6420 = ORIENTED_EDGE ( 'NONE', *, *, #4489, .F. ) ;
#6419 = EDGE_CURVE ( 'NONE', #19701, #23209, #23310, .T. ) ;
#6421 = ORIENTED_EDGE ( 'NONE', *, *, #10921, .F. ) ;
#6422 = ORIENTED_EDGE ( 'NONE', *, *, #12246, .F. ) ;
#6423 = VERTEX_POINT ( 'NONE', #9453 ) ;
#6424 = ORIENTED_EDGE ( 'NONE', *, *, #10475, .T. ) ;
#6425 = DIRECTION ( 'NONE',  ( 0.000000000000000000, -1.000000000000000000, 0.000000000000000000 ) ) ;
#6426 = EDGE_CURVE ( 'NONE', #6185, #6210, #19676, .T. ) ;
#6427 = MECHANICAL_DESIGN_GEOMETRIC_PRESENTATION_REPRESENTATION (  '', ( #16898 ), #6012 ) ;
#6428 = ORIENTED_EDGE ( 'NONE', *, *, #19749, .F. ) ;
#6429 = ADVANCED_FACE ( 'NONE', ( #19008 ), #23188, .F. ) ;
#6430 = DIRECTION ( 'NONE',  ( 1.000000000000000000, 0.000000000000000000, 0.000000000000000000 ) ) ;
#6431 = CARTESIAN_POINT ( 'NONE',  ( -3.756430356249996994, 25.92812499938548498, 8.999999999999992895 ) ) ;
#6432 = CARTESIAN_POINT ( 'NONE',  ( -3.756430356249996994, -8.999999999999992895, 3.628124999385483829 ) ) ;
#6433 = CARTESIAN_POINT ( 'NONE',  ( 3.469446951953614189E-15, 30.00000000000000355, 8.999999999999992895 ) ) ;
#6434 = CARTESIAN_POINT ( 'NONE',  ( 17.50966790313369259, 20.16586528109299437, 5.746835883940462963 ) ) ;
#6435 = EDGE_CURVE ( 'NONE', #20277, #8351, #25400, .T. ) ;
#6436 = DIRECTION ( 'NONE',  ( 0.5358267949790093132, 0.8443279255020070817, 0.000000000000000000 ) ) ;
#6437 = SURFACE_STYLE_USAGE ( .BOTH. , #42 ) ;
#6438 = CARTESIAN_POINT ( 'NONE',  ( 3.756430356250004099, -6.831223922626973533, 1.528124999385482186 ) ) ;
#6439 = CARTESIAN_POINT ( 'NONE',  ( -3.999999999999997335, 27.90624999877097068, 11.30940107675849404 ) ) ;
#6440 = CARTESIAN_POINT ( 'NONE',  ( -3.897863563849436552, 30.85476721088031482, -6.500000000000000000 ) ) ;
#6441 = CARTESIAN_POINT ( 'NONE',  ( -3.756430356249996994, 28.06562499938548427, 8.999999999999992895 ) ) ;
#6442 = CARTESIAN_POINT ( 'NONE',  ( 3.735045420075836212E-15, -4.662447845253954171, 3.065624999385482052 ) ) ;
#6443 = DIRECTION ( 'NONE',  ( -0.000000000000000000, -0.000000000000000000, -1.000000000000000000 ) ) ;
#6444 = CYLINDRICAL_SURFACE ( 'NONE', #14132, 4.000000000000000000 ) ;
#6445 = AXIS2_PLACEMENT_3D ( 'NONE', #12502, #8588, #16570 ) ;
#6446 = ORIENTED_EDGE ( 'NONE', *, *, #15233, .F. ) ;
#6447 = ORIENTED_EDGE ( 'NONE', *, *, #16714, .F. ) ;
#6448 = CARTESIAN_POINT ( 'NONE',  ( 3.756430356250002323, 28.44062499938549138, 6.831223922626973533 ) ) ;
#6449 = EDGE_LOOP ( 'NONE', ( #2809, #5671, #14464, #9784 ) ) ;
#6450 = FACE_OUTER_BOUND ( 'NONE', #4028, .T. ) ;
#6451 = ORIENTED_EDGE ( 'NONE', *, *, #20547, .F. ) ;
#6452 = CARTESIAN_POINT ( 'NONE',  ( 3.469446951953614189E-15, 38.49999999999999289, 8.999999999999992895 ) ) ;
#6453 = ORIENTED_EDGE ( 'NONE', *, *, #14801, .F. ) ;
#6454 = DIRECTION ( 'NONE',  ( 0.000000000000000000, 1.000000000000000000, 0.000000000000000000 ) ) ;
#6455 = ADVANCED_FACE ( 'NONE', ( #17049 ), #17319, .F. ) ;
#6456 = FACE_OUTER_BOUND ( 'NONE', #557, .T. ) ;
#6457 = VERTEX_POINT ( 'NONE', #7242 ) ;
#6458 = CARTESIAN_POINT ( 'NONE',  ( 2.000000000000003997, 28.61874999877096926, 5.535898384862238508 ) ) ;
#6459 = ADVANCED_FACE ( 'NONE', ( #2927 ), #15094, .F. ) ;
#6460 = CARTESIAN_POINT ( 'NONE',  ( -3.756430356249995661, 26.67812499938548498, 6.831223922626973533 ) ) ;
#6461 = DIRECTION ( 'NONE',  ( 0.000000000000000000, 0.000000000000000000, 1.000000000000000000 ) ) ;
#6462 = DIRECTION ( 'NONE',  ( 0.000000000000000000, 0.000000000000000000, 1.000000000000000000 ) ) ;
#6463 = DIRECTION ( 'NONE',  ( 0.000000000000000000, 0.000000000000000000, 1.000000000000000000 ) ) ;
#6464 = CARTESIAN_POINT ( 'NONE',  ( 0.000000000000000000, 28.93750000000000711, 13.61880215351699874 ) ) ;
#6465 = EDGE_CURVE ( 'NONE', #4650, #23081, #13132, .T. ) ;
#6466 = ADVANCED_FACE ( 'NONE', ( #23578 ), #7748, .F. ) ;
#6467 = CARTESIAN_POINT ( 'NONE',  ( 3.756430356250004099, 28.32812499938548356, 6.831223922626973533 ) ) ;
#6468 = CARTESIAN_POINT ( 'NONE',  ( 20.51285331117640709, 15.20045855525759393, 8.999999999999992895 ) ) ;
#6469 = VECTOR ( 'NONE', #15361, 1000.000000000000000 ) ;
#6470 = CARTESIAN_POINT ( 'NONE',  ( 5.706339097770919189, 29.50000000000000000, 7.145898033750285983 ) ) ;
#6471 = FACE_OUTER_BOUND ( 'NONE', #22077, .T. ) ;
#6472 = CARTESIAN_POINT ( 'NONE',  ( -3.756430356250002323, -26.00312499938548427, 11.16877607737301403 ) ) ;
#6473 = CYLINDRICAL_SURFACE ( 'NONE', #17536, 31.10000000000000142 ) ;
#6474 = EDGE_LOOP ( 'NONE', ( #18427, #12595, #14889 ) ) ;
#6475 = CARTESIAN_POINT ( 'NONE',  ( -1.878215178124995832, 25.40312499938548640, 5.746835883940462963 ) ) ;
#6476 = CARTESIAN_POINT ( 'NONE',  ( -2.000000000000000888, -28.97500000000000142, 12.46410161513774817 ) ) ;
#6478 = VERTEX_POINT ( 'NONE', #23447 ) ;
#6477 = CARTESIAN_POINT ( 'NONE',  ( -3.756430356249994329, 28.59062499938548996, 6.831223922626973533 ) ) ;
#6479 = VERTEX_POINT ( 'NONE', #5536 ) ;
#6480 = CARTESIAN_POINT ( 'NONE',  ( 3.999999999999997335, -29.25624999877096855, 11.30940107675849404 ) ) ;
#6481 = CARTESIAN_POINT ( 'NONE',  ( 3.818666391692735029, 38.64256296259726753, 4.558361811591131740 ) ) ;
#6482 = CARTESIAN_POINT ( 'NONE',  ( -3.999999999999996447, 25.61874999877096926, 8.999999999999992895 ) ) ;
#6483 = ORIENTED_EDGE ( 'NONE', *, *, #18211, .F. ) ;
#6484 = ORIENTED_EDGE ( 'NONE', *, *, #9563, .T. ) ;
#6485 = CARTESIAN_POINT ( 'NONE',  ( 3.756430356249996105, -25.89062499938548356, 6.831223922626973533 ) ) ;
#6486 = CARTESIAN_POINT ( 'NONE',  ( 1.878215178125001605, 27.31562499938548783, 12.25316411605952283 ) ) ;
#6487 = CARTESIAN_POINT ( 'NONE',  ( -4.000000000000001776, -28.95624999877097494, 11.30940107675849760 ) ) ;
#6488 = ADVANCED_FACE ( 'NONE', ( #4071 ), #13761, .F. ) ;
#6489 = CYLINDRICAL_SURFACE ( 'NONE', #10154, 4.000000000000000000 ) ;
#6490 = EDGE_CURVE ( 'NONE', #22605, #23233, #15922, .T. ) ;
#6491 = CARTESIAN_POINT ( 'NONE',  ( 21.96892380712053239, 19.14049668237426616, 5.535898384862238508 ) ) ;
#6492 =( LENGTH_UNIT ( ) NAMED_UNIT ( * ) SI_UNIT ( .MILLI., .METRE. ) );
#6493 = CARTESIAN_POINT ( 'NONE',  ( 0.000000000000000000, 0.000000000000000000, 15.00000000000000178 ) ) ;
#6494 = DIRECTION ( 'NONE',  ( -0.000000000000000000, -1.000000000000000000, -0.000000000000000000 ) ) ;
#6495 = DIRECTION ( 'NONE',  ( 0.000000000000000000, 0.000000000000000000, 1.000000000000000000 ) ) ;
#6496 = CARTESIAN_POINT ( 'NONE',  ( 21.99777755166815751, 16.68538279574934435, 11.16877607737301226 ) ) ;
#6497 = CARTESIAN_POINT ( 'NONE',  ( 17.92073748482754780, 20.74916460957366127, 5.535898384862237620 ) ) ;
#6498 = CARTESIAN_POINT ( 'NONE',  ( 4.000000000000001776, 27.66249999999999787, 11.30940107675849760 ) ) ;
#6499 = DIRECTION ( 'NONE',  ( 1.000000000000000000, 0.000000000000000000, 0.000000000000000000 ) ) ;
#6500 = CARTESIAN_POINT ( 'NONE',  ( 1.878215178125004048, 26.11562499938548498, 5.746835883940462963 ) ) ;
#6502 = ORIENTED_EDGE ( 'NONE', *, *, #11231, .T. ) ;
#6501 = DIRECTION ( 'NONE',  ( 1.000000000000000000, 0.000000000000000000, 0.000000000000000000 ) ) ;
#6503 = DIRECTION ( 'NONE',  ( -0.000000000000000000, -0.000000000000000000, -1.000000000000000000 ) ) ;
#6504 = CARTESIAN_POINT ( 'NONE',  ( 21.75237235625120036, 16.09551810675874961, 11.30940107675849760 ) ) ;
#6505 = AXIS2_PLACEMENT_3D ( 'NONE', #7206, #9298, #15190 ) ;
#6506 = ORIENTED_EDGE ( 'NONE', *, *, #1804, .T. ) ;
#6507 = DIRECTION ( 'NONE',  ( -0.000000000000000000, -0.000000000000000000, -1.000000000000000000 ) ) ;
#6508 = CARTESIAN_POINT ( 'NONE',  ( 0.000000000000000000, 0.000000000000000000, -6.500000000000000000 ) ) ;
#6509 = CARTESIAN_POINT ( 'NONE',  ( 3.756430356249996994, -26.26562499938548711, 8.999999999999992895 ) ) ;
#6511 = ORIENTED_EDGE ( 'NONE', *, *, #9258, .T. ) ;
#6510 = CARTESIAN_POINT ( 'NONE',  ( 17.11198410471449094, 19.94041122946061151, 12.46410161513774639 ) ) ;
#6512 = FACE_OUTER_BOUND ( 'NONE', #23813, .T. ) ;
#6513 = ORIENTED_EDGE ( 'NONE', *, *, #22970, .F. ) ;
#6514 = CARTESIAN_POINT ( 'NONE',  ( -1.878215178125004048, -25.21562499938548285, 5.746835883940462963 ) ) ;
#6515 = VERTEX_POINT ( 'NONE', #15857 ) ;
#6516 = ORIENTED_EDGE ( 'NONE', *, *, #23757, .F. ) ;
#6517 = DIRECTION ( 'NONE',  ( 1.000000000000000000, 0.000000000000000000, 0.000000000000000000 ) ) ;
#6518 = CARTESIAN_POINT ( 'NONE',  ( -1.499999999999998224, -10.49999999999999289, -6.938893903907228378E-15 ) ) ;
#6519 = CARTESIAN_POINT ( 'NONE',  ( 4.000000000000012434, -6.690598923241494411, 1.837499999999995914 ) ) ;
#6520 = EDGE_CURVE ( 'NONE', #20598, #3781, #22207, .T. ) ;
#6521 = CARTESIAN_POINT ( 'NONE',  ( 2.672651547586948120E-15, -13.33755215474602984, 1.040624999385485472 ) ) ;
#6522 =( LENGTH_UNIT ( ) NAMED_UNIT ( * ) SI_UNIT ( .MILLI., .METRE. ) );
#6523 = DIRECTION ( 'NONE',  ( 0.000000000000000000, 0.000000000000000000, 1.000000000000000000 ) ) ;
#6524 = CARTESIAN_POINT ( 'NONE',  ( -3.756430356249997882, 25.85312499938548925, 11.16877607737301226 ) ) ;
#6525 = EDGE_CURVE ( 'NONE', #5290, #23357, #10922, .T. ) ;
#6526 = CARTESIAN_POINT ( 'NONE',  ( 20.50609665440990526, 14.84924240491746339, 8.999999999999992895 ) ) ;
#6527 = CARTESIAN_POINT ( 'NONE',  ( 1.999999999999998224, -28.90000000000000213, 12.46410161513774639 ) ) ;
#6528 = CARTESIAN_POINT ( 'NONE',  ( -3.756430356249996994, 26.26562499938548711, 8.999999999999992895 ) ) ;
#6529 = CARTESIAN_POINT ( 'NONE',  ( 3.469446951953614189E-15, 35.50000000000000711, 8.999999999999992895 ) ) ;
#6530 = DIRECTION ( 'NONE',  ( -0.3681245526846659843, 0.9297764858882561212, 0.000000000000000000 ) ) ;
#6531 = CARTESIAN_POINT ( 'NONE',  ( -3.999999999999996447, 28.76874999877096784, 8.999999999999992895 ) ) ;
#6532 = CARTESIAN_POINT ( 'NONE',  ( 1.878215178124995832, -25.85312499938548569, 5.746835883940462963 ) ) ;
#6533 = CARTESIAN_POINT ( 'NONE',  ( -1.999999999999994893, 27.40000000000000213, 5.535898384862237620 ) ) ;
#6535 = ADVANCED_FACE ( 'NONE', ( #5658 ), #21489, .T. ) ;
#6534 = DIRECTION ( 'NONE',  ( -0.3681245526846659843, 0.9297764858882561212, 0.000000000000000000 ) ) ;
#6536 = LINE ( 'NONE', #6927, #25437 ) ;
#6537 = CARTESIAN_POINT ( 'NONE',  ( 2.004590926901224535, -29.93374515888019971, 5.528701699505815803 ) ) ;
#6538 = ORIENTED_EDGE ( 'NONE', *, *, #4434, .T. ) ;
#6539 = CARTESIAN_POINT ( 'NONE',  ( -14.98253926456298579, 27.25313774936435962, -6.500000000000000000 ) ) ;
#6541 = ORIENTED_EDGE ( 'NONE', *, *, #20248, .F. ) ;
#6540 = CARTESIAN_POINT ( 'NONE',  ( -3.469446951953614189E-15, -30.00000000000000355, 4.999999999999992006 ) ) ;
#6542 = VERTEX_POINT ( 'NONE', #13638 ) ;
#6543 = VERTEX_POINT ( 'NONE', #13902 ) ;
#6544 = ORIENTED_EDGE ( 'NONE', *, *, #14170, .F. ) ;
#6545 = ORIENTED_EDGE ( 'NONE', *, *, #5241, .F. ) ;
#6546 = ORIENTED_EDGE ( 'NONE', *, *, #23210, .T. ) ;
#6547 = DIRECTION ( 'NONE',  ( 1.000000000000000000, 0.000000000000000000, 0.000000000000000000 ) ) ;
#6548 = ORIENTED_EDGE ( 'NONE', *, *, #10109, .T. ) ;
#6549 = CARTESIAN_POINT ( 'NONE',  ( -27.10000000000000142, 0.000000000000000000, 0.000000000000000000 ) ) ;
#6550 = CARTESIAN_POINT ( 'NONE',  ( 0.000000000000000000, 0.000000000000000000, -6.500000000000000000 ) ) ;
#6551 =( BOUNDED_CURVE ( )  B_SPLINE_CURVE ( 2, ( #167, #17947, #23825, #33, #18326 ),
 .UNSPECIFIED., .F., .T. ) 
 B_SPLINE_CURVE_WITH_KNOTS ( ( 3, 2, 3 ),
 ( 0.9749999999999999778, 0.9833333333333332815, 0.9889400238386636399 ),
 .UNSPECIFIED. ) 
 CURVE ( )  GEOMETRIC_REPRESENTATION_ITEM ( )  RATIONAL_B_SPLINE_CURVE ( ( 0.9330127018922194093, 0.9330127018922194093, 1.000000000000000000, 0.9549307542065648136, 0.9401842259098239785 ) ) 
 REPRESENTATION_ITEM ( '' )  );
#6552 = CARTESIAN_POINT ( 'NONE',  ( 1.878215178125000939, -12.25316411605952283, 2.878124999385483385 ) ) ;
#6553 = DIRECTION ( 'NONE',  ( -0.000000000000000000, -1.000000000000000000, -0.000000000000000000 ) ) ;
#6554 = CARTESIAN_POINT ( 'NONE',  ( 21.36138144860026600, 16.04898669268145639, 11.16877607737301226 ) ) ;
#6555 = LINE ( 'NONE', #6684, #25090 ) ;
#6556 = ADVANCED_FACE ( 'NONE', ( #6045 ), #15124, .T. ) ;
#6557 = CARTESIAN_POINT ( 'NONE',  ( 1.701696020694480449, -26.00000000000000355, 20.00001200000000878 ) ) ;
#6558 = CONTEXT_DEPENDENT_SHAPE_REPRESENTATION ( #22119, #4637 ) ;
#6559 = CARTESIAN_POINT ( 'NONE',  ( 3.756430356250002323, -11.16877607737301226, 2.803124999385479210 ) ) ;
#6560 = CARTESIAN_POINT ( 'NONE',  ( -3.999999999999996447, -8.999999999999992895, 0.2249999999999995060 ) ) ;
#6561 = CARTESIAN_POINT ( 'NONE',  ( 2.000000000000000888, -12.46410161513774817, 3.974999999999999201 ) ) ;
#6562 = CARTESIAN_POINT ( 'NONE',  ( -1.499999999999998224, -7.499999999999992895, 30.00000000000000355 ) ) ;
#6563 = CARTESIAN_POINT ( 'NONE',  ( -3.756430356249996994, 29.41562499938548569, 8.999999999999992895 ) ) ;
#6564 = CARTESIAN_POINT ( 'NONE',  ( 2.672651547586948120E-15, -13.33755215474603162, 2.390624999385484450 ) ) ;
#6565 = EDGE_CURVE ( 'NONE', #19625, #18150, #11767, .T. ) ;
#6566 = CARTESIAN_POINT ( 'NONE',  ( 3.469446951953614189E-15, -8.999999999999992895, 18.00000000000000000 ) ) ;
#6567 = ORIENTED_EDGE ( 'NONE', *, *, #18928, .T. ) ;
#6568 = ORIENTED_EDGE ( 'NONE', *, *, #14610, .T. ) ;
#6569 = CARTESIAN_POINT ( 'NONE',  ( -3.756430356249998326, 28.66562499938548925, 11.16877607737301226 ) ) ;
#6570 = ORIENTED_EDGE ( 'NONE', *, *, #16093, .F. ) ;
#6571 = CARTESIAN_POINT ( 'NONE',  ( 3.834746474454188013E-15, 28.65624999877096712, 4.999999999999992006 ) ) ;
#6572 = VERTEX_POINT ( 'NONE', #868 ) ;
#6573 = DIRECTION ( 'NONE',  ( 0.000000000000000000, 0.000000000000000000, 1.000000000000000000 ) ) ;
#6574 = EDGE_CURVE ( 'NONE', #10324, #19323, #18037, .T. ) ;
#6575 = ORIENTED_EDGE ( 'NONE', *, *, #11151, .T. ) ;
#6576 = CARTESIAN_POINT ( 'NONE',  ( 0.000000000000000000, 0.000000000000000000, 15.00000000000000178 ) ) ;
#6577 = DIRECTION ( 'NONE',  ( 0.000000000000000000, 0.000000000000000000, 1.000000000000000000 ) ) ;
#6578 = ORIENTED_EDGE ( 'NONE', *, *, #15011, .F. ) ;
#6579 = CARTESIAN_POINT ( 'NONE',  ( -1.499999999999998224, -10.49999999999999289, 4.999999999999993783 ) ) ;
#6580 = CARTESIAN_POINT ( 'NONE',  ( -3.756430356249997882, 29.45312499938548356, 11.16877607737301226 ) ) ;
#6581 = CYLINDRICAL_SURFACE ( 'NONE', #23898, 31.10000000000000142 ) ;
#6582 = VECTOR ( 'NONE', #13913, 1000.000000000000000 ) ;
#6583 = DIRECTION ( 'NONE',  ( 0.000000000000000000, 1.000000000000000000, 0.000000000000000000 ) ) ;
#6584 = CARTESIAN_POINT ( 'NONE',  ( -1.999999999999998224, 26.65000000000000568, 12.46410161513774639 ) ) ;
#6585 = ADVANCED_FACE ( 'NONE', ( #14390 ), #16837, .F. ) ;
#6586 = CARTESIAN_POINT ( 'NONE',  ( 16.63462326141533865, 19.29082063937464397, 5.746835883940462963 ) ) ;
#6587 = CARTESIAN_POINT ( 'NONE',  ( 1.878215178125000939, 27.31562499938548427, 12.25316411605952283 ) ) ;
#6588 = ADVANCED_FACE ( 'NONE', ( #22839 ), #20125, .T. ) ;
#6589 = CARTESIAN_POINT ( 'NONE',  ( 20.80453485841585959, 15.49214010249704643, 11.16877607737301403 ) ) ;
#6590 = EDGE_CURVE ( 'NONE', #21352, #25423, #1759, .T. ) ;
#6591 = CARTESIAN_POINT ( 'NONE',  ( -3.999999999999999556, 26.03124999877097423, 6.690598923241487306 ) ) ;
#6592 = CARTESIAN_POINT ( 'NONE',  ( 20.87601458749065131, 19.36026505963852173, 12.99999999999998757 ) ) ;
#6593 = CARTESIAN_POINT ( 'NONE',  ( -1.878215178125000939, -27.76562499938548356, 12.25316411605952283 ) ) ;
#6594 = LINE ( 'NONE', #6208, #5816 ) ;
#6595 = ORIENTED_EDGE ( 'NONE', *, *, #17953, .F. ) ;
#6596 = CARTESIAN_POINT ( 'NONE',  ( -1.999999999999995781, 29.59374999877096712, 5.535898384862237620 ) ) ;
#6597 = CARTESIAN_POINT ( 'NONE',  ( -2.000000000000000888, -28.52500000000000213, 12.46410161513774817 ) ) ;
#6598 = EDGE_CURVE ( 'NONE', #14914, #5737, #6747, .T. ) ;
#6600 = ORIENTED_EDGE ( 'NONE', *, *, #6052, .T. ) ;
#6599 = CARTESIAN_POINT ( 'NONE',  ( 1.878215178125001605, 29.22812499938549280, 12.25316411605952283 ) ) ;
#6601 = ORIENTED_EDGE ( 'NONE', *, *, #12325, .T. ) ;
#6602 = DIRECTION ( 'NONE',  ( 1.000000000000000000, 0.000000000000000000, 0.000000000000000000 ) ) ;
#6603 = CIRCLE ( 'NONE', #2854, 0.4999999999999998890 ) ;
#6604 = ORIENTED_EDGE ( 'NONE', *, *, #12674, .T. ) ;
#6605 = CARTESIAN_POINT ( 'NONE',  ( -2.672651547586948120E-15, -26.94062499938548783, 13.33755215474603162 ) ) ;
#6606 = CARTESIAN_POINT ( 'NONE',  ( -1.878215178124999829, 27.69062499938549138, 12.25316411605951927 ) ) ;
#6607 = DIRECTION ( 'NONE',  ( 0.000000000000000000, -0.000000000000000000, 1.000000000000000000 ) ) ;
#6608 = CARTESIAN_POINT ( 'NONE',  ( 3.756430356250002323, -11.16877607737301403, 4.603124999385482141 ) ) ;
#6609 = CARTESIAN_POINT ( 'NONE',  ( -1.878215178124994722, 27.99062499938548143, 5.746835883940462963 ) ) ;
#6610 = AXIS2_PLACEMENT_3D ( 'NONE', #14274, #16610, #14517 ) ;
#6611 = CARTESIAN_POINT ( 'NONE',  ( 3.752267015613588906E-15, -4.381197846482986158, 3.262500000000001066 ) ) ;
#6612 = VECTOR ( 'NONE', #3479, 999.9999999999998863 ) ;
#6613 = DIRECTION ( 'NONE',  ( 1.000000000000000000, 0.000000000000000000, 0.000000000000000000 ) ) ;
#6614 = CARTESIAN_POINT ( 'NONE',  ( 18.73522341023428339, 20.25097293808625665, 12.99999999999999645 ) ) ;
#6615 = DIRECTION ( 'NONE',  ( 0.3681245526846875782, 0.9297764858882475725, 0.000000000000000000 ) ) ;
#6616 = CARTESIAN_POINT ( 'NONE',  ( -3.897863563849436552, 30.85476721088031482, 1.000000000000000000 ) ) ;
#6617 = VECTOR ( 'NONE', #19720, 1000.000000000000000 ) ;
#6618 = CARTESIAN_POINT ( 'NONE',  ( -19.82388608118446527, -23.96296185032687376, 1.000000000000000000 ) ) ;
#6619 = CARTESIAN_POINT ( 'NONE',  ( 16.87099832581089132, 22.18339308172956237, 8.999999999999992895 ) ) ;
#6620 = CARTESIAN_POINT ( 'NONE',  ( 23.30358785661013243, 17.64673360711768169, 11.30940107675849760 ) ) ;
#6621 = CARTESIAN_POINT ( 'NONE',  ( 2.000000000000000888, 27.62500000000000000, 12.46410161513774817 ) ) ;
#6622 = FACE_OUTER_BOUND ( 'NONE', #19495, .T. ) ;
#6623 = CARTESIAN_POINT ( 'NONE',  ( 3.735045420075836212E-15, 25.70312499938548001, 4.662447845253954171 ) ) ;
#6625 = VERTEX_POINT ( 'NONE', #18298 ) ;
#6624 = CARTESIAN_POINT ( 'NONE',  ( -30.91344420362549172, -3.401318489840897019, 1.000000000000000000 ) ) ;
#6626 = DIRECTION ( 'NONE',  ( 0.000000000000000000, 0.000000000000000000, -1.000000000000000000 ) ) ;
#6627 = CYLINDRICAL_SURFACE ( 'NONE', #3757, 4.000000000000000000 ) ;
#6628 = ORIENTED_EDGE ( 'NONE', *, *, #14268, .T. ) ;
#6629 = CARTESIAN_POINT ( 'NONE',  ( 3.469446951953614189E-15, -8.999999999999992895, 8.000000000000000000 ) ) ;
#6630 = CARTESIAN_POINT ( 'NONE',  ( 4.000000000000003553, 28.13124999877096855, 6.690598923241489970 ) ) ;
#6631 = CARTESIAN_POINT ( 'NONE',  ( -1.878215178125000939, -25.51562499938548356, 12.25316411605952283 ) ) ;
#6632 = EDGE_CURVE ( 'NONE', #11238, #19496, #21457, .T. ) ;
#6634 = ORIENTED_EDGE ( 'NONE', *, *, #9319, .F. ) ;
#6633 = CARTESIAN_POINT ( 'NONE',  ( 17.78062925563244079, 19.29637878348441404, 12.99999999999999467 ) ) ;
#6635 = DIRECTION ( 'NONE',  ( -1.000000000000000000, 0.000000000000000000, 0.000000000000000000 ) ) ;
#6636 = EDGE_CURVE ( 'NONE', #16757, #23529, #17218, .T. ) ;
#6637 = VECTOR ( 'NONE', #2173, 1000.000000000000000 ) ;
#6638 = ORIENTED_EDGE ( 'NONE', *, *, #13633, .T. ) ;
#6639 = CARTESIAN_POINT ( 'NONE',  ( 1.878215178124998497, -25.44062499938548427, 12.25316411605951927 ) ) ;
#6640 = ORIENTED_EDGE ( 'NONE', *, *, #12893, .F. ) ;
#6641 = ORIENTED_EDGE ( 'NONE', *, *, #21998, .F. ) ;
#6642 = CARTESIAN_POINT ( 'NONE',  ( -5.827558883616271501, -30.54913349766217934, 1.000000000000000000 ) ) ;
#6643 = EDGE_CURVE ( 'NONE', #15394, #17898, #2044, .T. ) ;
#6644 = CARTESIAN_POINT ( 'NONE',  ( 3.756430356250002323, 26.11562499938549564, 11.16877607737301226 ) ) ;
#6645 = AXIS2_PLACEMENT_3D ( 'NONE', #10080, #24549, #6635 ) ;
#6646 = ADVANCED_FACE ( 'NONE', ( #21798 ), #7797, .F. ) ;
#6647 = CIRCLE ( 'NONE', #16269, 0.4999999999999993894 ) ;
#6648 = CARTESIAN_POINT ( 'NONE',  ( -3.999999999999996447, -8.999999999999992895, 3.318749998770968102 ) ) ;
#6649 = CARTESIAN_POINT ( 'NONE',  ( -1.878215178124998497, -12.25316411605951927, 1.903124999385483296 ) ) ;
#6650 = CARTESIAN_POINT ( 'NONE',  ( 21.83060874209248325, 20.31485921424036434, 12.99999999999999467 ) ) ;
#6651 = COLOUR_RGB ( '',0.8941176470588234615, 0.8941176470588234615, 0.8941176470588234615 ) ;
#6652 = CARTESIAN_POINT ( 'NONE',  ( 3.756430356250003655, 26.49062499938548498, 8.999999999999992895 ) ) ;
#6653 = CARTESIAN_POINT ( 'NONE',  ( 17.75721904254721295, 17.75721904254714545, 4.999999999999992006 ) ) ;
#6654 = AXIS2_PLACEMENT_3D ( 'NONE', #8607, #18558, #2597 ) ;
#6655 = DIRECTION ( 'NONE',  ( 0.000000000000000000, 0.000000000000000000, 1.000000000000000000 ) ) ;
#6656 = CARTESIAN_POINT ( 'NONE',  ( 3.756430356250002323, 27.80312499938548143, 11.16877607737301403 ) ) ;
#6657 = CARTESIAN_POINT ( 'NONE',  ( 21.21320343559646915, 21.21320343559638744, 12.99999999999999289 ) ) ;
#6658 = CARTESIAN_POINT ( 'NONE',  ( -0.4999838450259764255, 31.09598070739550124, 1.000000000000000000 ) ) ;
#6659 = CARTESIAN_POINT ( 'NONE',  ( 16.79378605318053985, 19.62221317792666753, 12.46410161513774639 ) ) ;
#6660 = CARTESIAN_POINT ( 'NONE',  ( -3.756430356250003655, -26.15312499938548640, 8.999999999999992895 ) ) ;
#6661 = CARTESIAN_POINT ( 'NONE',  ( -7.734255490827218971, -30.12293631110037140, -6.500000000000000000 ) ) ;
#6662 = DIRECTION ( 'NONE',  ( 1.000000000000000000, 0.000000000000000000, 0.000000000000000000 ) ) ;
#6663 = DIRECTION ( 'NONE',  ( 0.000000000000000000, -0.000000000000000000, 1.000000000000000000 ) ) ;
#6664 = CARTESIAN_POINT ( 'NONE',  ( 3.871726839561290490, -29.74915783848840434, 10.03836643961818886 ) ) ;
#6665 = ORIENTED_EDGE ( 'NONE', *, *, #17800, .F. ) ;
#6666 = DIRECTION ( 'NONE',  ( 0.000000000000000000, 0.000000000000000000, 1.000000000000000000 ) ) ;
#6668 = ORIENTED_EDGE ( 'NONE', *, *, #5952, .F. ) ;
#6667 = CARTESIAN_POINT ( 'NONE',  ( 4.000000000000003553, -8.999999999999992895, 3.543749998770967302 ) ) ;
#6669 = EDGE_CURVE ( 'NONE', #23121, #20602, #23055, .T. ) ;
#6670 = EDGE_LOOP ( 'NONE', ( #9857, #20964, #21991, #10810 ) ) ;
#6671 = VERTEX_POINT ( 'NONE', #17482 ) ;
#6672 = VERTEX_POINT ( 'NONE', #10012 ) ;
#6673 = VERTEX_POINT ( 'NONE', #7675 ) ;
#6674 = CARTESIAN_POINT ( 'NONE',  ( 25.99519186311192342, 0.5000000000000000000, 20.00000000000000000 ) ) ;
#6675 = AXIS2_PLACEMENT_3D ( 'NONE', #21199, #3277, #11250 ) ;
#6676 = VERTEX_POINT ( 'NONE', #21533 ) ;
#6677 = CARTESIAN_POINT ( 'NONE',  ( 23.64116323484238080, 20.20656826142275264, -2.750000000000000000 ) ) ;
#6678 = CARTESIAN_POINT ( 'NONE',  ( -3.756430356249997438, 29.11562499938548498, 11.16877607737301048 ) ) ;
#6679 = VECTOR ( 'NONE', #6553, 1000.000000000000000 ) ;
#6680 = EDGE_CURVE ( 'NONE', #4728, #4688, #19267, .T. ) ;
#6681 = CARTESIAN_POINT ( 'NONE',  ( -3.756430356249996994, -8.999999999999992895, 1.828124999385484450 ) ) ;
#6682 = DIRECTION ( 'NONE',  ( 0.000000000000000000, 0.000000000000000000, 1.000000000000000000 ) ) ;
#6683 = CARTESIAN_POINT ( 'NONE',  ( 22.68720666332504621, 17.37481190740622239, 6.831223922626973533 ) ) ;
#6684 = CARTESIAN_POINT ( 'NONE',  ( -3.999999999999996447, -8.999999999999992895, 18.00000000000000000 ) ) ;
#6685 = CARTESIAN_POINT ( 'NONE',  ( -1.701696020694465128, -26.00000000000001066, 20.00001200000000878 ) ) ;
#6686 = CARTESIAN_POINT ( 'NONE',  ( 1.878215178125000939, -12.25316411605952283, 2.315624999385482941 ) ) ;
#6687 = DIRECTION ( 'NONE',  ( 0.000000000000000000, 0.000000000000000000, 1.000000000000000000 ) ) ;
#6688 = CARTESIAN_POINT ( 'NONE',  ( 3.752267015613588906E-15, -4.381197846482986158, 3.262500000000001066 ) ) ;
#6689 = FACE_OUTER_BOUND ( 'NONE', #19441, .T. ) ;
#6690 = DIRECTION ( 'NONE',  ( 0.000000000000000000, -0.000000000000000000, -1.000000000000000000 ) ) ;
#6691 = AXIS2_PLACEMENT_3D ( 'NONE', #12016, #2355, #20133 ) ;
#6692 = CARTESIAN_POINT ( 'NONE',  ( 3.756430356250002323, -11.16877607737301403, 2.465624999385482852 ) ) ;
#6693 = AXIS2_PLACEMENT_3D ( 'NONE', #5197, #22853, #7288 ) ;
#6694 = CARTESIAN_POINT ( 'NONE',  ( 2.000000000000005329, 25.46874999877096712, 5.535898384862238508 ) ) ;
#6695 = DIRECTION ( 'NONE',  ( 0.000000000000000000, 0.000000000000000000, -1.000000000000000000 ) ) ;
#6696 = ORIENTED_EDGE ( 'NONE', *, *, #4698, .T. ) ;
#6697 = ORIENTED_EDGE ( 'NONE', *, *, #23757, .T. ) ;
#6698 = CARTESIAN_POINT ( 'NONE',  ( 3.756430356250004543, 28.89062499938549067, 6.831223922626973533 ) ) ;
#6699 = AXIS2_PLACEMENT_3D ( 'NONE', #8537, #20684, #8928 ) ;
#6700 = EDGE_LOOP ( 'NONE', ( #15869, #6600, #24648, #23026 ) ) ;
#6701 = CARTESIAN_POINT ( 'NONE',  ( 4.000000000000003553, 25.00000000000000000, 8.999999999999992895 ) ) ;
#6702 = ORIENTED_EDGE ( 'NONE', *, *, #20767, .F. ) ;
#6703 = CARTESIAN_POINT ( 'NONE',  ( 3.756430356249997882, -25.51562499938548356, 11.16877607737301226 ) ) ;
#6704 = ORIENTED_EDGE ( 'NONE', *, *, #18730, .F. ) ;
#6705 = LINE ( 'NONE', #16652, #2162 ) ;
#6706 = VECTOR ( 'NONE', #4126, 1000.000000000000000 ) ;
#6707 = VERTEX_POINT ( 'NONE', #15776 ) ;
#6708 = EDGE_CURVE ( 'NONE', #10320, #21754, #10085, .T. ) ;
#6709 = DIRECTION ( 'NONE',  ( -0.000000000000000000, -1.000000000000000000, -0.000000000000000000 ) ) ;
#6710 = CARTESIAN_POINT ( 'NONE',  ( 2.000000000000003997, 25.52500000000000213, 5.535898384862238508 ) ) ;
#6711 = DIRECTION ( 'NONE',  ( 1.000000000000000000, 0.000000000000000000, 0.000000000000000000 ) ) ;
#6712 = AXIS2_PLACEMENT_3D ( 'NONE', #14512, #20258, #22233 ) ;
#6713 = AXIS2_PLACEMENT_3D ( 'NONE', #23451, #11542, #7752 ) ;
#6714 = DIRECTION ( 'NONE',  ( 1.387778780781445044E-14, 1.000000000000000000, 0.000000000000000000 ) ) ;
#6715 = CARTESIAN_POINT ( 'NONE',  ( 29.72853858738285737, 9.133673601486364646, -2.750000000000000000 ) ) ;
#6716 = CARTESIAN_POINT ( 'NONE',  ( 18.22561351908507277, 20.88181089704437454, 5.746835883940462963 ) ) ;
#6717 = CIRCLE ( 'NONE', #2136, 0.4999999999999991118 ) ;
#6718 = EDGE_CURVE ( 'NONE', #23467, #19338, #5587, .T. ) ;
#6719 = CIRCLE ( 'NONE', #5466, 0.4999999999999991118 ) ;
#6720 = CARTESIAN_POINT ( 'NONE',  ( 1.878215178125004048, 28.81562499938548427, 5.746835883940462963 ) ) ;
#6721 = CARTESIAN_POINT ( 'NONE',  ( 19.44991966514168169, 16.79372228718224491, 12.25316411605952283 ) ) ;
#6722 = CARTESIAN_POINT ( 'NONE',  ( -23.01025686871616216, 20.92219106202074741, -2.750000000000000000 ) ) ;
#6723 = CIRCLE ( 'NONE', #10898, 31.10000000000000142 ) ;
#6724 = CARTESIAN_POINT ( 'NONE',  ( 0.000000000000000000, 0.000000000000000000, 1.000000000000000000 ) ) ;
#6725 = PRODUCT_DEFINITION_SHAPE ( 'NONE', 'NONE',  #25885 ) ;
#6726 = CARTESIAN_POINT ( 'NONE',  ( 4.000000000000000888, 26.25624999877096144, 11.30940107675849760 ) ) ;
#6727 = CARTESIAN_POINT ( 'NONE',  ( 0.000000000000000000, 10.00000000000000000, 13.00000000000000178 ) ) ;
#6728 = CARTESIAN_POINT ( 'NONE',  ( -3.735045420075836212E-15, -27.50312499938548427, 4.662447845253954171 ) ) ;
#6729 = AXIS2_PLACEMENT_3D ( 'NONE', #18439, #19574, #11094 ) ;
#6730 = CARTESIAN_POINT ( 'NONE',  ( 5.840899737312979845, 38.49999999999999289, 10.37254881831474052 ) ) ;
#6731 = ORIENTED_EDGE ( 'NONE', *, *, #21422, .F. ) ;
#6732 = CARTESIAN_POINT ( 'NONE',  ( 3.756430356250004099, 25.29062499938548569, 6.831223922626973533 ) ) ;
#6733 = EDGE_CURVE ( 'NONE', #23985, #7474, #20545, .T. ) ;
#6734 = CARTESIAN_POINT ( 'NONE',  ( -30.35476721088022600, 3.897863563850190616, -6.500000000000000000 ) ) ;
#6736 = ORIENTED_EDGE ( 'NONE', *, *, #5664, .F. ) ;
#6735 = CARTESIAN_POINT ( 'NONE',  ( 3.756430356250000546, 29.26562499938548356, 11.16877607737301403 ) ) ;
#6737 = ORIENTED_EDGE ( 'NONE', *, *, #23613, .F. ) ;
#6738 = CARTESIAN_POINT ( 'NONE',  ( 3.999999999999996447, -29.21874999877096712, 8.999999999999992895 ) ) ;
#6739 = AXIS2_PLACEMENT_3D ( 'NONE', #9995, #17989, #4107 ) ;
#6740 = EDGE_CURVE ( 'NONE', #13215, #364, #23865, .T. ) ;
#6741 = DIRECTION ( 'NONE',  ( -0.000000000000000000, -1.000000000000000000, -0.000000000000000000 ) ) ;
#6742 = ORIENTED_EDGE ( 'NONE', *, *, #14143, .F. ) ;
#6743 = CARTESIAN_POINT ( 'NONE',  ( 1.878215178124995832, -25.85312499938548569, 5.746835883940462963 ) ) ;
#6744 = CARTESIAN_POINT ( 'NONE',  ( 7.734255490827002255, 30.12293631110042469, -6.500000000000000000 ) ) ;
#6745 = CARTESIAN_POINT ( 'NONE',  ( -3.756430356249996549, 25.32812499938548356, 6.831223922626973533 ) ) ;
#6746 = ADVANCED_FACE ( 'NONE', ( #9637, #23626 ), #15914, .T. ) ;
#6747 = CIRCLE ( 'NONE', #14289, 0.4999999999999997224 ) ;
#6748 = DIRECTION ( 'NONE',  ( 0.000000000000000000, 0.000000000000000000, -1.000000000000000000 ) ) ;
#6749 = CARTESIAN_POINT ( 'NONE',  ( 3.756430356250004543, 26.07812499938549422, 6.831223922626973533 ) ) ;
#6750 = EDGE_CURVE ( 'NONE', #15121, #9972, #13030, .T. ) ;
#6751 = AXIS2_PLACEMENT_3D ( 'NONE', #10640, #22300, #18634 ) ;
#6752 = CIRCLE ( 'NONE', #5503, 0.5000000000000002220 ) ;
#6753 = DIRECTION ( 'NONE',  ( 0.000000000000000000, -1.000000000000000000, 0.000000000000000000 ) ) ;
#6754 = EDGE_CURVE ( 'NONE', #17713, #6479, #15660, .T. ) ;
#6755 = FACE_BOUND ( 'NONE', #21088, .T. ) ;
#6756 = AXIS2_PLACEMENT_3D ( 'NONE', #12326, #24965, #17000 ) ;
#6757 = DIRECTION ( 'NONE',  ( 0.8763066800438640280, -0.4817536741017146018, 0.000000000000000000 ) ) ;
#6758 = CARTESIAN_POINT ( 'NONE',  ( 0.5000000000000000000, -2.999999999999999556, 19.50000000000000000 ) ) ;
#6759 = DIRECTION ( 'NONE',  ( 1.000000000000000000, 0.000000000000000000, 0.000000000000000000 ) ) ;
#6760 = CARTESIAN_POINT ( 'NONE',  ( 20.11283227250407180, 17.45663489454462436, 5.746835883940462963 ) ) ;
#6761 = CARTESIAN_POINT ( 'NONE',  ( 20.80453485841585959, 15.49214010249704643, 11.16877607737301226 ) ) ;
#6762 = DIRECTION ( 'NONE',  ( 0.000000000000000000, -0.000000000000000000, 1.000000000000000000 ) ) ;
#6763 = DIRECTION ( 'NONE',  ( 0.000000000000000000, -0.000000000000000000, 1.000000000000000000 ) ) ;
#6764 = CARTESIAN_POINT ( 'NONE',  ( 1.878215178125004048, 27.01562499938548711, 5.746835883940462963 ) ) ;
#6766 = VERTEX_POINT ( 'NONE', #19700 ) ;
#6765 = DIRECTION ( 'NONE',  ( -0.000000000000000000, 0.000000000000000000, -1.000000000000000000 ) ) ;
#6767 = CIRCLE ( 'NONE', #95, 0.5000000000000003331 ) ;
#6768 = DIRECTION ( 'NONE',  ( 0.7071067811865487940, 0.7071067811865463515, 0.000000000000000000 ) ) ;
#6769 = DIRECTION ( 'NONE',  ( 0.000000000000000000, 0.000000000000000000, -1.000000000000000000 ) ) ;
#6770 = ORIENTED_EDGE ( 'NONE', *, *, #9923, .F. ) ;
#6771 = CARTESIAN_POINT ( 'NONE',  ( 3.756430356250004987, 29.69687499938549280, 8.999999999999992895 ) ) ;
#6772 = CARTESIAN_POINT ( 'NONE',  ( 2.000000000000000888, 28.91874999877096997, 12.46410161513774817 ) ) ;
#6773 = CARTESIAN_POINT ( 'NONE',  ( -3.756430356250004099, -26.52812499938548285, 6.831223922626973533 ) ) ;
#6775 = ORIENTED_EDGE ( 'NONE', *, *, #15340, .T. ) ;
#6774 = CARTESIAN_POINT ( 'NONE',  ( -1.999999999999998224, 25.69374999877097210, 12.46410161513774639 ) ) ;
#6776 = VECTOR ( 'NONE', #59, 1000.000000000000000 ) ;
#6777 = LINE ( 'NONE', #20895, #16672 ) ;
#6778 = CIRCLE ( 'NONE', #5932, 0.4999999999999998890 ) ;
#6779 = ORIENTED_EDGE ( 'NONE', *, *, #12019, .T. ) ;
#6780 = CARTESIAN_POINT ( 'NONE',  ( -3.756430356250003655, -26.04062499938548569, 8.999999999999992895 ) ) ;
#6781 = ORIENTED_EDGE ( 'NONE', *, *, #12288, .T. ) ;
#6782 = ORIENTED_EDGE ( 'NONE', *, *, #22216, .F. ) ;
#6783 = DIRECTION ( 'NONE',  ( 0.000000000000000000, 0.000000000000000000, 1.000000000000000000 ) ) ;
#6785 = CARTESIAN_POINT ( 'NONE',  ( 3.756430356250002323, 27.46562499938548640, 11.16877607737301226 ) ) ;
#6784 = AXIS2_PLACEMENT_3D ( 'NONE', #22959, #733, #19153 ) ;
#6786 = DIRECTION ( 'NONE',  ( 0.000000000000000000, 0.000000000000000000, 1.000000000000000000 ) ) ;
#6787 =( BOUNDED_CURVE ( )  B_SPLINE_CURVE ( 2, ( #5137, #14818, #16783, #8938, #22791, #9176, #5378, #17168, #6835 ),
 .UNSPECIFIED., .F., .F. ) 
 B_SPLINE_CURVE_WITH_KNOTS ( ( 3, 2, 2, 2, 3 ),
 ( 0.3250000000000000111, 0.3333333333333333148, 0.3499999999999999778, 0.3666666666666666408, 0.3750000000000000000 ),
 .UNSPECIFIED. ) 
 CURVE ( )  GEOMETRIC_REPRESENTATION_ITEM ( )  RATIONAL_B_SPLINE_CURVE ( ( 0.9330127018922194093, 0.9330127018922196314, 1.000000000000000000, 0.8660254037844387076, 1.000000000000000000, 0.8660254037844387076, 1.000000000000000000, 0.9330127018922194093, 0.9330127018922194093 ) ) 
 REPRESENTATION_ITEM ( '' )  );
#6788 = CARTESIAN_POINT ( 'NONE',  ( -3.756430356249996994, -8.999999999999992895, 1.828124999385484450 ) ) ;
#6789 = EDGE_CURVE ( 'NONE', #25495, #10104, #24297, .T. ) ;
#6790 = CARTESIAN_POINT ( 'NONE',  ( -3.202926563175272801, 39.00162299460587434, 4.530527552673861535 ) ) ;
#6791 = CARTESIAN_POINT ( 'NONE',  ( 3.756430356250002323, 29.60312499938548569, 11.16877607737301226 ) ) ;
#6792 = EDGE_CURVE ( 'NONE', #23568, #14371, #4658, .T. ) ;
#6793 = VECTOR ( 'NONE', #14276, 1000.000000000000000 ) ;
#6794 = CARTESIAN_POINT ( 'NONE',  ( 2.000000000000003997, -5.535898384862238508, 1.818749998770966769 ) ) ;
#6795 = CARTESIAN_POINT ( 'NONE',  ( 3.110308778861350820, 31.50000000000000000, 14.13088484572962855 ) ) ;
#6796 = UNCERTAINTY_MEASURE_WITH_UNIT (LENGTH_MEASURE( 1.000000000000000082E-05 ), #9926, 'distance_accuracy_value', 'NONE');
#6797 = PRODUCT_DEFINITION_CONTEXT ( 'detailed design', #8614, 'design' ) ;
#6798 = DIRECTION ( 'NONE',  ( 0.000000000000000000, 0.000000000000000000, -1.000000000000000000 ) ) ;
#6799 = CARTESIAN_POINT ( 'NONE',  ( 19.01364670445742888, 20.52939623230939858, 12.99999999999999645 ) ) ;
#6800 = CARTESIAN_POINT ( 'NONE',  ( -27.25313774936430633, -14.98253926456308172, 1.000000000000000000 ) ) ;
#6801 = DIRECTION ( 'NONE',  ( -0.7071067811865487940, -0.7071067811865463515, 0.000000000000000000 ) ) ;
#6802 = CARTESIAN_POINT ( 'NONE',  ( -3.735045420075836212E-15, -27.61562499938548498, 4.662447845253954171 ) ) ;
#6803 = DIRECTION ( 'NONE',  ( 0.000000000000000000, 0.000000000000000000, 1.000000000000000000 ) ) ;
#6804 = LINE ( 'NONE', #16885, #12892 ) ;
#6805 = DIRECTION ( 'NONE',  ( 1.000000000000000000, 0.000000000000000000, 0.000000000000000000 ) ) ;
#6806 = DIRECTION ( 'NONE',  ( 0.000000000000000000, 0.000000000000000000, 1.000000000000000000 ) ) ;
#6807 = ORIENTED_EDGE ( 'NONE', *, *, #13641, .T. ) ;
#6808 = FACE_OUTER_BOUND ( 'NONE', #24296, .T. ) ;
#6810 = VERTEX_POINT ( 'NONE', #3741 ) ;
#6809 = DIRECTION ( 'NONE',  ( 0.000000000000000000, 0.000000000000000000, 1.000000000000000000 ) ) ;
#6811 = AXIS2_PLACEMENT_3D ( 'NONE', #25307, #7385, #17074 ) ;
#6812 = ORIENTED_EDGE ( 'NONE', *, *, #23697, .F. ) ;
#6813 = ORIENTED_EDGE ( 'NONE', *, *, #9008, .F. ) ;
#6814 = ORIENTED_EDGE ( 'NONE', *, *, #12872, .T. ) ;
#6815 = ORIENTED_EDGE ( 'NONE', *, *, #24365, .T. ) ;
#6816 = CARTESIAN_POINT ( 'NONE',  ( 3.469446951953614189E-15, 30.00000000000000355, 8.999999999999992895 ) ) ;
#6817 = VECTOR ( 'NONE', #13979, 1000.000000000000000 ) ;
#6818 = ORIENTED_EDGE ( 'NONE', *, *, #18931, .F. ) ;
#6819 = CARTESIAN_POINT ( 'NONE',  ( 4.000000000000001776, 29.50000000000000711, 8.999999999999992895 ) ) ;
#6820 = CARTESIAN_POINT ( 'NONE',  ( 3.756430356250003655, 28.40312499938548640, 8.999999999999992895 ) ) ;
#6821 = CIRCLE ( 'NONE', #17674, 0.5000000000000005551 ) ;
#6822 = EDGE_CURVE ( 'NONE', #21568, #19382, #7180, .T. ) ;
#6823 = CARTESIAN_POINT ( 'NONE',  ( -3.756430356249997882, -11.16877607737301226, 0.8531249993854844726 ) ) ;
#6824 = CARTESIAN_POINT ( 'NONE',  ( 3.469446951953614189E-15, 40.00000000000000000, 4.999999999999992006 ) ) ;
#6825 = DIRECTION ( 'NONE',  ( -0.000000000000000000, -1.000000000000000000, -0.000000000000000000 ) ) ;
#6826 = CARTESIAN_POINT ( 'NONE',  ( -1.878215178124998497, 26.00312499938548783, 12.25316411605951927 ) ) ;
#6827 = EDGE_CURVE ( 'NONE', #10501, #476, #18773, .T. ) ;
#6828 = DIRECTION ( 'NONE',  ( -0.000000000000000000, 1.000000000000000000, -0.000000000000000000 ) ) ;
#6829 = CARTESIAN_POINT ( 'NONE',  ( 1.878215178125000939, -12.25316411605952283, 3.665624999385483473 ) ) ;
#6830 = CARTESIAN_POINT ( 'NONE',  ( 1.533898589781675205E-14, 27.98124999877097352, 12.99999999999999289 ) ) ;
#6831 = CARTESIAN_POINT ( 'NONE',  ( -3.999999999999996003, -6.690598923241487306, 3.787499999999998757 ) ) ;
#6832 = CARTESIAN_POINT ( 'NONE',  ( -3.999999999999998224, 28.76874999877097139, 8.999999999999992895 ) ) ;
#6833 = FACE_OUTER_BOUND ( 'NONE', #13337, .T. ) ;
#6834 = CARTESIAN_POINT ( 'NONE',  ( -1.878215178124998497, -12.25316411605951927, 2.353124999385485694 ) ) ;
#6835 = CARTESIAN_POINT ( 'NONE',  ( -1.859271017917182139E-15, -26.68750000000000000, 12.99999999999999289 ) ) ;
#6836 = CARTESIAN_POINT ( 'NONE',  ( 3.469446951953614189E-15, 35.50000000000000711, 4.999999999999992006 ) ) ;
#6837 = EDGE_LOOP ( 'NONE', ( #24164, #1700, #16785, #17966 ) ) ;
#6838 = ORIENTED_EDGE ( 'NONE', *, *, #11478, .T. ) ;
#6839 = CARTESIAN_POINT ( 'NONE',  ( 3.756430356250006319, 27.09062499938548285, 6.831223922626973533 ) ) ;
#6840 = EDGE_CURVE ( 'NONE', #1348, #24947, #9767, .T. ) ;
#6841 = EDGE_LOOP ( 'NONE', ( #12278, #4608, #16264, #18489 ) ) ;
#6842 = DIRECTION ( 'NONE',  ( 0.000000000000000000, 0.000000000000000000, 1.000000000000000000 ) ) ;
#6843 = ORIENTED_EDGE ( 'NONE', *, *, #21664, .T. ) ;
#6844 = CARTESIAN_POINT ( 'NONE',  ( -3.735045420075836212E-15, -25.36562499938548498, 4.662447845253954171 ) ) ;
#6845 = ORIENTED_EDGE ( 'NONE', *, *, #19639, .T. ) ;
#6846 = DIRECTION ( 'NONE',  ( 0.000000000000000000, 0.000000000000000000, 1.000000000000000000 ) ) ;
#6847 = CIRCLE ( 'NONE', #5595, 0.4999999999999991118 ) ;
#6848 = ORIENTED_EDGE ( 'NONE', *, *, #6110, .T. ) ;
#6849 = DIRECTION ( 'NONE',  ( -0.7071067811865487940, -0.7071067811865463515, 0.000000000000000000 ) ) ;
#6850 = CARTESIAN_POINT ( 'NONE',  ( 3.756430356250004099, 29.22812499938548925, 6.831223922626973533 ) ) ;
#6851 = CARTESIAN_POINT ( 'NONE',  ( 1.999999999999995781, -27.40000000000000213, 5.535898384862237620 ) ) ;
#6852 = CARTESIAN_POINT ( 'NONE',  ( -30.63887302793251521, -5.335677986744475021, -2.750000000000000000 ) ) ;
#6853 = CARTESIAN_POINT ( 'NONE',  ( 17.32411613907045478, 20.15254326381657535, 5.535898384862237620 ) ) ;
#6854 = CARTESIAN_POINT ( 'NONE',  ( 18.41350252340144422, 18.41350252340138383, 13.33755215474602984 ) ) ;
#6855 = EDGE_CURVE ( 'NONE', #4270, #6478, #6705, .T. ) ;
#6856 = MECHANICAL_DESIGN_GEOMETRIC_PRESENTATION_REPRESENTATION (  '', ( #15619 ), #24816 ) ;
#6857 = CARTESIAN_POINT ( 'NONE',  ( -3.756430356249996994, 27.61562499938548143, 8.999999999999992895 ) ) ;
#6858 = EDGE_CURVE ( 'NONE', #6625, #13467, #7092, .T. ) ;
#6859 = CARTESIAN_POINT ( 'NONE',  ( -19.82388608118395013, 23.96296185032730364, 1.000000000000000000 ) ) ;
#6860 = CARTESIAN_POINT ( 'NONE',  ( 17.91631806831418317, 17.91631806831411566, 12.99999999999999289 ) ) ;
#6861 = ORIENTED_EDGE ( 'NONE', *, *, #15696, .T. ) ;
#6862 = DIRECTION ( 'NONE',  ( 1.000000000000000000, 0.000000000000000000, 0.000000000000000000 ) ) ;
#6863 = CARTESIAN_POINT ( 'NONE',  ( -3.999999999999996447, 26.55624999877097281, 11.30940107675849404 ) ) ;
#6864 = CARTESIAN_POINT ( 'NONE',  ( 1.878215178124995832, -26.64062499938548711, 5.746835883940462963 ) ) ;
#6865 = EDGE_CURVE ( 'NONE', #19049, #8071, #5497, .T. ) ;
#6866 = CARTESIAN_POINT ( 'NONE',  ( 8.217531866531214035, 29.99470236596028982, -2.750000000000000000 ) ) ;
#6867 = CARTESIAN_POINT ( 'NONE',  ( 2.000000000000003997, 29.51874999877096784, 5.535898384862238508 ) ) ;
#6868 = DIRECTION ( 'NONE',  ( 0.000000000000000000, 0.000000000000000000, 1.000000000000000000 ) ) ;
#6870 = ORIENTED_EDGE ( 'NONE', *, *, #2406, .T. ) ;
#6869 = CARTESIAN_POINT ( 'NONE',  ( 3.756430356250003211, 28.85312499938548569, 8.999999999999992895 ) ) ;
#6871 = ORIENTED_EDGE ( 'NONE', *, *, #6822, .T. ) ;
#6872 = CARTESIAN_POINT ( 'NONE',  ( 3.834746474454188013E-15, 28.65624999877096712, 4.999999999999992006 ) ) ;
#6873 = CARTESIAN_POINT ( 'NONE',  ( 3.897863563849651936, -30.85476721088028640, -6.500000000000000000 ) ) ;
#6874 = EDGE_LOOP ( 'NONE', ( #25657, #669 ) ) ;
#6875 = CARTESIAN_POINT ( 'NONE',  ( 1.878215178124995832, -29.45312499938548356, 5.746835883940462963 ) ) ;
#6876 = DIRECTION ( 'NONE',  ( 0.000000000000000000, 0.000000000000000000, 1.000000000000000000 ) ) ;
#6877 = CARTESIAN_POINT ( 'NONE',  ( -1.878215178124998275, 26.79062499938548569, 12.25316411605951927 ) ) ;
#6878 = CARTESIAN_POINT ( 'NONE',  ( 1.500000000000001776, -7.499999999999993783, -6.938893903907228378E-15 ) ) ;
#6879 = CARTESIAN_POINT ( 'NONE',  ( -3.756430356249996105, 28.47812499938548569, 6.831223922626973533 ) ) ;
#6880 = DIRECTION ( 'NONE',  ( 0.2486898871648653975, 0.9685831611286285225, 0.000000000000000000 ) ) ;
#6881 = CARTESIAN_POINT ( 'NONE',  ( 4.000000000000003553, -8.999999999999992895, 3.149999999999999911 ) ) ;
#6882 = SURFACE_STYLE_USAGE ( .BOTH. , #8708 ) ;
#6883 = FACE_OUTER_BOUND ( 'NONE', #18836, .T. ) ;
#6884 = CARTESIAN_POINT ( 'NONE',  ( -1.499999999999998224, -10.49999999999999289, 4.999999999999993783 ) ) ;
#6885 = ADVANCED_FACE ( 'NONE', ( #14700 ), #967, .T. ) ;
#6886 = CARTESIAN_POINT ( 'NONE',  ( 11.91206721063051432, 28.72825533807128551, -6.500000000000000000 ) ) ;
#6887 = DIRECTION ( 'NONE',  ( 0.000000000000000000, 0.000000000000000000, 1.000000000000000000 ) ) ;
#6888 = CARTESIAN_POINT ( 'NONE',  ( 20.85081121023835138, 15.19395696074590241, 6.690598923241489970 ) ) ;
#6889 = CARTESIAN_POINT ( 'NONE',  ( 21.44093096148375466, 16.12853620556493794, 11.16877607737301226 ) ) ;
#6890 = FACE_BOUND ( 'NONE', #24975, .T. ) ;
#6891 = PLANE ( 'NONE',  #16754 ) ;
#6892 = CARTESIAN_POINT ( 'NONE',  ( -3.756430356249996994, 28.51562499938548356, 8.999999999999992895 ) ) ;
#6894 = EDGE_CURVE ( 'NONE', #18387, #12818, #11335, .T. ) ;
#6893 = DIRECTION ( 'NONE',  ( 0.000000000000000000, 0.000000000000000000, 1.000000000000000000 ) ) ;
#6895 = CARTESIAN_POINT ( 'NONE',  ( 3.469446951953614189E-15, 25.00000000000000000, 8.999999999999992895 ) ) ;
#6896 = ORIENTED_EDGE ( 'NONE', *, *, #1789, .T. ) ;
#6897 = CARTESIAN_POINT ( 'NONE',  ( -3.999999999999996447, 28.82499999999999929, 8.999999999999992895 ) ) ;
#6898 = CARTESIAN_POINT ( 'NONE',  ( 4.000000000000001776, 28.50624999877096855, 11.30940107675849760 ) ) ;
#6899 = CARTESIAN_POINT ( 'NONE',  ( 3.756430356249995661, -29.37812499938548427, 6.831223922626973533 ) ) ;
#6901 = EDGE_LOOP ( 'NONE', ( #23596, #22832, #7859, #24550, #11914, #10464, #7157, #23330, #6390 ) ) ;
#6900 = CARTESIAN_POINT ( 'NONE',  ( -25.16042852506104666, -18.28012134629567598, 1.000000000000000000 ) ) ;
#6902 = DIRECTION ( 'NONE',  ( 0.8443279255020154084, -0.5358267949789962126, 0.000000000000000000 ) ) ;
#6903 = ORIENTED_EDGE ( 'NONE', *, *, #4530, .T. ) ;
#6904 = CARTESIAN_POINT ( 'NONE',  ( 1.878215178124998497, -28.59062499938548285, 12.25316411605951927 ) ) ;
#6905 = ORIENTED_EDGE ( 'NONE', *, *, #17877, .T. ) ;
#6906 = ADVANCED_FACE ( 'NONE', ( #4765 ), #75, .T. ) ;
#6907 = ORIENTED_EDGE ( 'NONE', *, *, #17726, .F. ) ;
#6908 = DIRECTION ( 'NONE',  ( 0.000000000000000000, 0.000000000000000000, 1.000000000000000000 ) ) ;
#6909 = CARTESIAN_POINT ( 'NONE',  ( -3.756430356249994329, 26.79062499938549280, 6.831223922626973533 ) ) ;
#6910 = CARTESIAN_POINT ( 'NONE',  ( -14.98253926456356666, -27.25313774936403988, -6.500000000000000000 ) ) ;
#6911 = CARTESIAN_POINT ( 'NONE',  ( 3.756430356250003655, -8.999999999999992895, 2.953124999385485339 ) ) ;
#6912 = SURFACE_STYLE_USAGE ( .BOTH. , #15024 ) ;
#6913 = EDGE_CURVE ( 'NONE', #16170, #12311, #7100, .T. ) ;
#6914 = CARTESIAN_POINT ( 'NONE',  ( -3.434389267989125027, 38.94985767598075910, 4.639816847356652119 ) ) ;
#6915 = CARTESIAN_POINT ( 'NONE',  ( 1.878215178125004048, 28.81562499938548427, 5.746835883940462963 ) ) ;
#6916 = CARTESIAN_POINT ( 'NONE',  ( 19.14491610062580662, 16.31648897587954750, 5.535898384862238508 ) ) ;
#6917 = DIRECTION ( 'NONE',  ( 1.000000000000000000, 0.000000000000000000, 0.000000000000000000 ) ) ;
#6918 = VECTOR ( 'NONE', #1177, 1000.000000000000000 ) ;
#6919 = CARTESIAN_POINT ( 'NONE',  ( -3.756430356249996994, 28.51562499938548356, 8.999999999999992895 ) ) ;
#6920 = CARTESIAN_POINT ( 'NONE',  ( 19.82388608118411710, -23.96296185032715798, 1.000000000000000000 ) ) ;
#6921 = CARTESIAN_POINT ( 'NONE',  ( 3.834746474454188013E-15, 25.95624999877096428, 4.999999999999992006 ) ) ;
#6922 = CARTESIAN_POINT ( 'NONE',  ( 4.000000000000003553, -8.999999999999992895, 0.8437499987709664584 ) ) ;
#6923 = CARTESIAN_POINT ( 'NONE',  ( 21.21320343559646915, 21.21320343559638744, 8.999999999999992895 ) ) ;
#6924 = CARTESIAN_POINT ( 'NONE',  ( -3.756430356250004099, -26.19062499938548783, 6.831223922626973533 ) ) ;
#6925 = CARTESIAN_POINT ( 'NONE',  ( -3.756430356249997882, 25.96562499938548640, 11.16877607737301226 ) ) ;
#6926 = CARTESIAN_POINT ( 'NONE',  ( 3.878215178125003604, 29.57031249969274356, 8.999999999999992895 ) ) ;
#6927 = CARTESIAN_POINT ( 'NONE',  ( 22.32573188046904633, -21.65113613650351709, -2.750000000000000000 ) ) ;
#6928 = CARTESIAN_POINT ( 'NONE',  ( 21.58443449571939965, 18.75600737097314052, 12.46410161513774817 ) ) ;
#6929 =( REPRESENTATION_RELATIONSHIP ('NONE','NONE', #25031, #4483 ) REPRESENTATION_RELATIONSHIP_WITH_TRANSFORMATION ( #5922 )SHAPE_REPRESENTATION_RELATIONSHIP( ) );
#6930 = ORIENTED_EDGE ( 'NONE', *, *, #2909, .F. ) ;
#6931 = AXIS2_PLACEMENT_3D ( 'NONE', #18042, #4418, #20497 ) ;
#6932 = DIRECTION ( 'NONE',  ( -0.7071067811865487940, -0.7071067811865463515, 0.000000000000000000 ) ) ;
#6934 = VERTEX_POINT ( 'NONE', #24764 ) ;
#6933 = DIRECTION ( 'NONE',  ( -0.8763066800438656934, -0.4817536741017116597, 0.000000000000000000 ) ) ;
#6935 = EDGE_CURVE ( 'NONE', #18179, #25045, #16534, .T. ) ;
#6936 =( BOUNDED_CURVE ( )  B_SPLINE_CURVE ( 2, ( #23137, #21049, #9653, #21428, #1676, #17121, #1290, #3375, #19071 ),
 .UNSPECIFIED., .F., .F. ) 
 B_SPLINE_CURVE_WITH_KNOTS ( ( 3, 2, 2, 2, 3 ),
 ( 0.8750000000000000000, 0.8833333333333333037, 0.9000000000000000222, 0.9166666666666666297, 0.9250000000000000444 ),
 .UNSPECIFIED. ) 
 CURVE ( )  GEOMETRIC_REPRESENTATION_ITEM ( )  RATIONAL_B_SPLINE_CURVE ( ( 0.9330127018922194093, 0.9330127018922194093, 1.000000000000000000, 0.8660254037844387076, 1.000000000000000000, 0.8660254037844387076, 1.000000000000000000, 0.9330127018922189652, 0.9330127018922194093 ) ) 
 REPRESENTATION_ITEM ( '' )  );
#6937 = EDGE_LOOP ( 'NONE', ( #3883, #24733, #5771, #1346 ) ) ;
#6938 = VERTEX_POINT ( 'NONE', #14556 ) ;
#6939 = VERTEX_POINT ( 'NONE', #4879 ) ;
#6940 = ADVANCED_FACE ( 'NONE', ( #12854 ), #20828, .F. ) ;
#6941 = EDGE_LOOP ( 'NONE', ( #15565, #25746, #7742, #3457, #17141, #3836 ) ) ;
#6942 = LINE ( 'NONE', #6674, #16399 ) ;
#6943 =( BOUNDED_CURVE ( )  B_SPLINE_CURVE ( 2, ( #19813, #25581, #5695, #13674, #3728, #11712, #19689, #7787, #9248 ),
 .UNSPECIFIED., .F., .T. ) 
 B_SPLINE_CURVE_WITH_KNOTS ( ( 3, 2, 2, 2, 3 ),
 ( 0.3750000000000000000, 0.3833333333333333592, 0.4000000000000000222, 0.4166666666666666852, 0.4250000000000000444 ),
 .UNSPECIFIED. ) 
 CURVE ( )  GEOMETRIC_REPRESENTATION_ITEM ( )  RATIONAL_B_SPLINE_CURVE ( ( 0.9330127018922194093, 0.9330127018922194093, 1.000000000000000000, 0.8660254037844387076, 1.000000000000000000, 0.8660254037844387076, 1.000000000000000000, 0.9330127018922191873, 0.9330127018922194093 ) ) 
 REPRESENTATION_ITEM ( '' )  );
#6944 = ADVANCED_FACE ( 'NONE', ( #18879 ), #2665, .F. ) ;
#6945 = EDGE_LOOP ( 'NONE', ( #1371, #24611, #1738 ) ) ;
#6946 = LINE ( 'NONE', #8920, #21956 ) ;
#6947 = CARTESIAN_POINT ( 'NONE',  ( 3.756430356250003655, 29.75312499938548783, 8.999999999999992895 ) ) ;
#6948 = CARTESIAN_POINT ( 'NONE',  ( 3.735045420075836212E-15, -4.662447845253954171, 0.2531249993854848279 ) ) ;
#6949 = LINE ( 'NONE', #562, #23796 ) ;
#6950 = CARTESIAN_POINT ( 'NONE',  ( 22.95237170627000367, 17.63997695035117985, 11.16877607737301226 ) ) ;
#6951 = CARTESIAN_POINT ( 'NONE',  ( 1.878215178125004048, 25.77812499938548640, 5.746835883940462963 ) ) ;
#6952 = CARTESIAN_POINT ( 'NONE',  ( 2.000000000000003997, -5.535898384862238508, 0.5250000000000011324 ) ) ;
#6953 = CARTESIAN_POINT ( 'NONE',  ( 3.756430356250004099, -6.831223922626973533, 4.228124999385484806 ) ) ;
#6954 = DIRECTION ( 'NONE',  ( 1.000000000000000000, -0.000000000000000000, -0.000000000000000000 ) ) ;
#6955 = CARTESIAN_POINT ( 'NONE',  ( -3.999999999999996447, -8.999999999999992895, 3.374999999999999556 ) ) ;
#6956 = CARTESIAN_POINT ( 'NONE',  ( 18.98139765660737055, 21.80982478135348757, 12.46410161513774639 ) ) ;
#6957 = CARTESIAN_POINT ( 'NONE',  ( -26.25859848311282363, -16.66421332384654974, -6.500000000000000000 ) ) ;
#6958 = CARTESIAN_POINT ( 'NONE',  ( -1.878215178124995832, -5.746835883940462963, 4.003124999385484273 ) ) ;
#6959 = CYLINDRICAL_SURFACE ( 'NONE', #12874, 0.5000000000000004441 ) ;
#6960 = CARTESIAN_POINT ( 'NONE',  ( -2.000000000000000888, -25.37500000000000000, 12.46410161513774817 ) ) ;
#6961 = ORIENTED_EDGE ( 'NONE', *, *, #1682, .T. ) ;
#6962 = ORIENTED_EDGE ( 'NONE', *, *, #22803, .T. ) ;
#6963 = ORIENTED_EDGE ( 'NONE', *, *, #19852, .F. ) ;
#6964 = FACE_OUTER_BOUND ( 'NONE', #545, .T. ) ;
#6965 = ORIENTED_EDGE ( 'NONE', *, *, #10618, .F. ) ;
#6966 = CARTESIAN_POINT ( 'NONE',  ( -3.756430356250003655, -25.70312499938548356, 8.999999999999992895 ) ) ;
#6967 = ADVANCED_FACE ( 'NONE', ( #23062 ), #18498, .F. ) ;
#6968 = VERTEX_POINT ( 'NONE', #586 ) ;
#6969 = DIRECTION ( 'NONE',  ( 0.000000000000000000, -0.000000000000000000, 1.000000000000000000 ) ) ;
#6970 = EDGE_CURVE ( 'NONE', #9505, #25113, #8434, .T. ) ;
#6971 = ORIENTED_EDGE ( 'NONE', *, *, #25063, .T. ) ;
#6972 = DIRECTION ( 'NONE',  ( 0.000000000000000000, 0.000000000000000000, 1.000000000000000000 ) ) ;
#6973 = CARTESIAN_POINT ( 'NONE',  ( 1.878215178125004048, 29.26562499938548356, 5.746835883940462963 ) ) ;
#6974 = ADVANCED_FACE ( 'NONE', ( #22536, #4618 ), #10627, .T. ) ;
#6975 = CARTESIAN_POINT ( 'NONE',  ( 2.000000000000003997, 27.26874999877097139, 5.535898384862238508 ) ) ;
#6976 = FACE_OUTER_BOUND ( 'NONE', #15743, .T. ) ;
#6977 = CARTESIAN_POINT ( 'NONE',  ( 3.469446951953614189E-15, -8.999999999999992895, 18.00000000000000000 ) ) ;
#6978 = CARTESIAN_POINT ( 'NONE',  ( 22.44855812467459089, 17.13616336875576351, 6.831223922626973533 ) ) ;
#6979 = DIRECTION ( 'NONE',  ( 1.000000000000000000, 0.000000000000000000, 0.000000000000000000 ) ) ;
#6980 = CARTESIAN_POINT ( 'NONE',  ( 2.000000000000000888, 25.37500000000000000, 12.46410161513774817 ) ) ;
#6981 = CARTESIAN_POINT ( 'NONE',  ( 17.58921741601718125, 20.24541479397648303, 5.746835883940462963 ) ) ;
#6982 = DIRECTION ( 'NONE',  ( 0.000000000000000000, -1.000000000000000000, 0.000000000000000000 ) ) ;
#6983 = VERTEX_POINT ( 'NONE', #19253 ) ;
#6984 = CARTESIAN_POINT ( 'NONE',  ( 4.000000000000005329, 28.09374999877097778, 8.999999999999992895 ) ) ;
#6985 = CARTESIAN_POINT ( 'NONE',  ( -1.878215178125000939, -28.21562499938548640, 12.25316411605952283 ) ) ;
#6986 = CARTESIAN_POINT ( 'NONE',  ( 8.831537335106614961E-15, 27.13750000000000284, 12.99999999999999112 ) ) ;
#6987 = CARTESIAN_POINT ( 'NONE',  ( -3.999999999999997335, 29.70624999877097139, 11.30940107675849404 ) ) ;
#6988 = DIRECTION ( 'NONE',  ( 1.000000000000000000, -0.000000000000000000, -0.000000000000000000 ) ) ;
#6990 = EDGE_LOOP ( 'NONE', ( #13780, #1474, #5491, #16402 ) ) ;
#6989 = CARTESIAN_POINT ( 'NONE',  ( -1.878215178124996498, 29.00312499938548783, 5.746835883940462963 ) ) ;
#6991 = ADVANCED_FACE ( 'NONE', ( #25394 ), #7236, .F. ) ;
#6992 = ORIENTED_EDGE ( 'NONE', *, *, #21739, .F. ) ;
#6993 = FACE_OUTER_BOUND ( 'NONE', #24232, .T. ) ;
#6994 = EDGE_CURVE ( 'NONE', #1492, #24730, #25148, .T. ) ;
#6995 = CARTESIAN_POINT ( 'NONE',  ( -9.133673601486059113, 29.72853858738294619, -2.750000000000000000 ) ) ;
#6996 = ORIENTED_EDGE ( 'NONE', *, *, #1068, .F. ) ;
#6997 = CARTESIAN_POINT ( 'NONE',  ( 3.756430356250003655, 29.75312499938548783, 8.999999999999992895 ) ) ;
#6998 = CARTESIAN_POINT ( 'NONE',  ( -1.452785157361865531, -31.03863125411923463, -6.500000000000000000 ) ) ;
#6999 = CARTESIAN_POINT ( 'NONE',  ( -3.756430356250000546, 26.30312499938548854, 11.16877607737301048 ) ) ;
#7000 = DIRECTION ( 'NONE',  ( 0.2486898871648519360, -0.9685831611286318532, 0.000000000000000000 ) ) ;
#7001 = CARTESIAN_POINT ( 'NONE',  ( 3.756430356250002323, 28.32812499938549067, 6.831223922626973533 ) ) ;
#7002 = EDGE_CURVE ( 'NONE', #5585, #2254, #9190, .T. ) ;
#7003 = CARTESIAN_POINT ( 'NONE',  ( 5.706339097770919189, 31.50000000000000000, 7.145898033750285983 ) ) ;
#7004 =( NAMED_UNIT ( * ) PLANE_ANGLE_UNIT ( ) SI_UNIT ( $, .RADIAN. ) );
#7005 = CARTESIAN_POINT ( 'NONE',  ( 20.58122674904192451, 20.58122674904186411, 4.999999999999992006 ) ) ;
#7006 = CYLINDRICAL_SURFACE ( 'NONE', #2157, 31.10000000000000142 ) ;
#7007 = AXIS2_PLACEMENT_3D ( 'NONE', #4998, #20961, #11397 ) ;
#7008 = CARTESIAN_POINT ( 'NONE',  ( -3.756430356249996105, 28.02812499938548996, 6.831223922626973533 ) ) ;
#7009 = CARTESIAN_POINT ( 'NONE',  ( -3.834746474454188013E-15, -28.20624999877096428, 4.999999999999992006 ) ) ;
#7010 = CARTESIAN_POINT ( 'NONE',  ( 20.40224034548861809, 20.40224034548853638, 4.662447845253954171 ) ) ;
#7011 = CARTESIAN_POINT ( 'NONE',  ( 17.93620544610052647, 17.93620544610046252, 4.662447845253954171 ) ) ;
#7012 = CARTESIAN_POINT ( 'NONE',  ( 0.000000000000000000, 0.000000000000000000, -6.500000000000000000 ) ) ;
#7013 = CARTESIAN_POINT ( 'NONE',  ( -3.756430356249995661, 28.92812499938548143, 6.831223922626973533 ) ) ;
#7014 = CARTESIAN_POINT ( 'NONE',  ( 23.77396755978151077, 18.29757075420054235, 7.964378325765101962 ) ) ;
#7015 = CARTESIAN_POINT ( 'NONE',  ( 21.70609600442870857, 16.39370124850988830, 8.999999999999992895 ) ) ;
#7016 = DIRECTION ( 'NONE',  ( 0.000000000000000000, 1.000000000000000000, 0.000000000000000000 ) ) ;
#7017 = AXIS2_PLACEMENT_3D ( 'NONE', #22355, #20525, #4439 ) ;
#7018 = ORIENTED_EDGE ( 'NONE', *, *, #24863, .F. ) ;
#7019 = CARTESIAN_POINT ( 'NONE',  ( -21.28941499438242246, -22.67092431280570963, -6.500000000000000000 ) ) ;
#7020 = CARTESIAN_POINT ( 'NONE',  ( -1.999999999999998224, 28.84374999877096712, 12.46410161513774639 ) ) ;
#7021 = CARTESIAN_POINT ( 'NONE',  ( -3.756430356250002323, -29.15312499938548640, 11.16877607737301226 ) ) ;
#7023 = ORIENTED_EDGE ( 'NONE', *, *, #8660, .F. ) ;
#7022 = DIRECTION ( 'NONE',  ( -0.8763066800438602533, 0.4817536741017213187, 0.000000000000000000 ) ) ;
#7024 = CARTESIAN_POINT ( 'NONE',  ( 3.756430356250003655, 25.25312499938548427, 8.999999999999992895 ) ) ;
#7025 = ORIENTED_EDGE ( 'NONE', *, *, #15570, .T. ) ;
#7026 = CARTESIAN_POINT ( 'NONE',  ( -1.878215178125000939, -27.76562499938548356, 12.25316411605952283 ) ) ;
#7027 = ORIENTED_EDGE ( 'NONE', *, *, #25200, .T. ) ;
#7028 = ORIENTED_EDGE ( 'NONE', *, *, #18367, .F. ) ;
#7029 = CARTESIAN_POINT ( 'NONE',  ( 20.46846337105369074, 21.93416294652367426, 5.127803451112006528 ) ) ;
#7030 = CARTESIAN_POINT ( 'NONE',  ( 6.009258394948636914E-15, 27.61562499938548854, 4.662447845253954171 ) ) ;
#7031 = AXIS2_PLACEMENT_3D ( 'NONE', #19342, #11491, #19463 ) ;
#7032 = ADVANCED_FACE ( 'NONE', ( #1351 ), #19633, .T. ) ;
#7033 = DIRECTION ( 'NONE',  ( 0.000000000000000000, 0.000000000000000000, 1.000000000000000000 ) ) ;
#7034 = AXIS2_PLACEMENT_3D ( 'NONE', #18111, #24491, #18227 ) ;
#7035 = VECTOR ( 'NONE', #7184, 1000.000000000000000 ) ;
#7036 = CARTESIAN_POINT ( 'NONE',  ( 3.756430356250003655, -8.999999999999992895, 4.303124999385482319 ) ) ;
#7037 = EDGE_CURVE ( 'NONE', #21732, #5974, #2165, .T. ) ;
#7038 = CARTESIAN_POINT ( 'NONE',  ( -3.338796519864625445, 38.98631256281465340, 4.611909993434559318 ) ) ;
#7039 = CARTESIAN_POINT ( 'NONE',  ( 1.878215178125000939, 28.66562499938548569, 12.25316411605952283 ) ) ;
#7040 = CARTESIAN_POINT ( 'NONE',  ( 0.000000000000000000, 0.000000000000000000, -6.500000000000000000 ) ) ;
#7041 = CARTESIAN_POINT ( 'NONE',  ( -14.98253926456356666, -27.25313774936403988, -6.500000000000000000 ) ) ;
#7042 = UNCERTAINTY_MEASURE_WITH_UNIT (LENGTH_MEASURE( 1.000000000000000082E-05 ), #11728, 'distance_accuracy_value', 'NONE');
#7043 = PRODUCT_DEFINITION_CONTEXT ( 'detailed design', #24801, 'design' ) ;
#7044 = CARTESIAN_POINT ( 'NONE',  ( -1.878215178124998497, 29.49062499938548498, 12.25316411605951927 ) ) ;
#7045 = DIRECTION ( 'NONE',  ( 0.000000000000000000, 0.000000000000000000, 1.000000000000000000 ) ) ;
#7046 = LINE ( 'NONE', #9400, #13722 ) ;
#7047 = CARTESIAN_POINT ( 'NONE',  ( 0.000000000000000000, 0.000000000000000000, -6.500000000000000000 ) ) ;
#7048 = CARTESIAN_POINT ( 'NONE',  ( 0.000000000000000000, 0.000000000000000000, 1.000000000000000000 ) ) ;
#7049 = CARTESIAN_POINT ( 'NONE',  ( -3.735045420075836212E-15, -26.71562499938548640, 4.662447845253954171 ) ) ;
#7050 = CARTESIAN_POINT ( 'NONE',  ( 3.878215178125003604, -8.999999999999992895, 0.3234374990782259984 ) ) ;
#7051 = CARTESIAN_POINT ( 'NONE',  ( -1.057460391440397258E-14, 29.55624999877096926, 4.999999999999992006 ) ) ;
#7052 = AXIS2_PLACEMENT_3D ( 'NONE', #21524, #21788, #15381 ) ;
#7053 = CARTESIAN_POINT ( 'NONE',  ( -3.999999999999996447, 26.06874999877096855, 8.999999999999992895 ) ) ;
#7054 = CARTESIAN_POINT ( 'NONE',  ( -1.057460391440397258E-14, 29.16249999999999787, 4.999999999999992006 ) ) ;
#7056 = VERTEX_POINT ( 'NONE', #23688 ) ;
#7055 = AXIS2_PLACEMENT_3D ( 'NONE', #5573, #21519, #5308 ) ;
#7057 = CARTESIAN_POINT ( 'NONE',  ( -5.500712606062064580, 38.82887297708774810, 7.617000894021300539 ) ) ;
#7059 = ORIENTED_EDGE ( 'NONE', *, *, #7653, .T. ) ;
#7058 = PLANE ( 'NONE',  #3716 ) ;
#7060 = AXIS2_PLACEMENT_3D ( 'NONE', #16560, #12762, #4385 ) ;
#7061 = ORIENTED_EDGE ( 'NONE', *, *, #19431, .F. ) ;
#7062 = ORIENTED_EDGE ( 'NONE', *, *, #17841, .F. ) ;
#7063 = ORIENTED_EDGE ( 'NONE', *, *, #10001, .F. ) ;
#7064 = ORIENTED_EDGE ( 'NONE', *, *, #15329, .F. ) ;
#7065 = LINE ( 'NONE', #23158, #11791 ) ;
#7066 = CARTESIAN_POINT ( 'NONE',  ( 3.469446951953614189E-15, -8.999999999999992895, 18.00000000000000000 ) ) ;
#7067 = ORIENTED_EDGE ( 'NONE', *, *, #8131, .T. ) ;
#7068 = DIRECTION ( 'NONE',  ( 0.000000000000000000, 0.000000000000000000, 1.000000000000000000 ) ) ;
#7069 = EDGE_CURVE ( 'NONE', #23065, #13512, #5404, .T. ) ;
#7070 = AXIS2_PLACEMENT_3D ( 'NONE', #9670, #21952, #13713 ) ;
#7071 = CARTESIAN_POINT ( 'NONE',  ( 3.756430356250003655, -8.999999999999992895, 1.040624999385484584 ) ) ;
#7072 =( NAMED_UNIT ( * ) SI_UNIT ( $, .STERADIAN. ) SOLID_ANGLE_UNIT ( ) );
#7073 = CARTESIAN_POINT ( 'NONE',  ( 0.7500000000000001110, 1.299038105676658450, 18.19999999999999929 ) ) ;
#7074 = EDGE_CURVE ( 'NONE', #8556, #19701, #13454, .T. ) ;
#7075 = FACE_OUTER_BOUND ( 'NONE', #16434, .T. ) ;
#7076 = AXIS2_PLACEMENT_3D ( 'NONE', #11923, #10091, #8143 ) ;
#7077 = CARTESIAN_POINT ( 'NONE',  ( 23.36965697125208408, -11.52193136556784658, 20.00001200000000168 ) ) ;
#7078 = VECTOR ( 'NONE', #2298, 1000.000000000000000 ) ;
#7079 = CARTESIAN_POINT ( 'NONE',  ( -3.756430356249997882, -11.16877607737301226, 4.003124999385478056 ) ) ;
#7080 = CARTESIAN_POINT ( 'NONE',  ( 3.918623196469491976, 38.49999999999999289, 13.54361004533742907 ) ) ;
#7082 = ADVANCED_FACE ( 'NONE', ( #11533 ), #11410, .T. ) ;
#7081 = CARTESIAN_POINT ( 'NONE',  ( -1.952785157361865753, -31.03863125411923463, -6.500000000000000000 ) ) ;
#7083 = DIRECTION ( 'NONE',  ( -0.000000000000000000, 1.000000000000000000, -0.000000000000000000 ) ) ;
#7084 =( BOUNDED_CURVE ( )  B_SPLINE_CURVE ( 2, ( #12351, #8565, #14454, #8821, #10514, #22815, #20316, #20191, #4775 ),
 .UNSPECIFIED., .F., .F. ) 
 B_SPLINE_CURVE_WITH_KNOTS ( ( 3, 2, 2, 2, 3 ),
 ( 0.2250000000000000056, 0.2333333333333333370, 0.2500000000000000000, 0.2666666666666666630, 0.2750000000000000222 ),
 .UNSPECIFIED. ) 
 CURVE ( )  GEOMETRIC_REPRESENTATION_ITEM ( )  RATIONAL_B_SPLINE_CURVE ( ( 0.9330127018922194093, 0.9330127018922194093, 1.000000000000000000, 0.8660254037844387076, 1.000000000000000000, 0.8660254037844387076, 1.000000000000000000, 0.9330127018922191873, 0.9330127018922194093 ) ) 
 REPRESENTATION_ITEM ( '' )  );
#7085 = CARTESIAN_POINT ( 'NONE',  ( 4.143002691484658293E-15, 46.00000000000000000, 14.49999999999999289 ) ) ;
#7086 = CARTESIAN_POINT ( 'NONE',  ( 1.878215178125000939, -12.25316411605952283, 4.678124999385483207 ) ) ;
#7087 = DIRECTION ( 'NONE',  ( 0.000000000000000000, 0.000000000000000000, 1.000000000000000000 ) ) ;
#7088 = AXIS2_PLACEMENT_3D ( 'NONE', #20724, #10767, #1469 ) ;
#7089 = CARTESIAN_POINT ( 'NONE',  ( 8.831537335106614961E-15, 27.53124999877097068, 12.99999999999999112 ) ) ;
#7090 = VERTEX_POINT ( 'NONE', #13632 ) ;
#7091 = ORIENTED_EDGE ( 'NONE', *, *, #1628, .T. ) ;
#7092 =( BOUNDED_CURVE ( )  B_SPLINE_CURVE ( 2, ( #2917, #704, #8805, #20577, #10497, #25011, #16924, #9059, #10749 ),
 .UNSPECIFIED., .F., .F. ) 
 B_SPLINE_CURVE_WITH_KNOTS ( ( 3, 2, 2, 2, 3 ),
 ( 0.5250000000000000222, 0.5333333333333333259, 0.5500000000000000444, 0.5666666666666666519, 0.5750000000000000666 ),
 .UNSPECIFIED. ) 
 CURVE ( )  GEOMETRIC_REPRESENTATION_ITEM ( )  RATIONAL_B_SPLINE_CURVE ( ( 0.9330127018922194093, 0.9330127018922194093, 1.000000000000000000, 0.8660254037844387076, 1.000000000000000000, 0.8660254037844387076, 1.000000000000000000, 0.9330127018922189652, 0.9330127018922194093 ) ) 
 REPRESENTATION_ITEM ( '' )  );
#7093 = AXIS2_PLACEMENT_3D ( 'NONE', #12645, #16841, #10930 ) ;
#7095 = ORIENTED_EDGE ( 'NONE', *, *, #23089, .T. ) ;
#7094 = CIRCLE ( 'NONE', #13775, 0.4999999999999991673 ) ;
#7096 = DIRECTION ( 'NONE',  ( -0.8660254037844397068, -0.4999999999999983347, 0.000000000000000000 ) ) ;
#7097 = VERTEX_POINT ( 'NONE', #3173 ) ;
#7098 = CARTESIAN_POINT ( 'NONE',  ( -2.672651547586948120E-15, -25.59062499938548640, 13.33755215474602984 ) ) ;
#7099 = ORIENTED_EDGE ( 'NONE', *, *, #5478, .T. ) ;
#7100 = LINE ( 'NONE', #22802, #14694 ) ;
#7101 = AXIS2_PLACEMENT_3D ( 'NONE', #8013, #18091, #17820 ) ;
#7102 = CIRCLE ( 'NONE', #2504, 31.10000000000000142 ) ;
#7103 = VERTEX_POINT ( 'NONE', #13245 ) ;
#7104 = CARTESIAN_POINT ( 'NONE',  ( 0.000000000000000000, 0.000000000000000000, -6.500000000000000000 ) ) ;
#7105 = CARTESIAN_POINT ( 'NONE',  ( 1.878215178125000939, 28.66562499938548569, 12.25316411605952283 ) ) ;
#7106 = CARTESIAN_POINT ( 'NONE',  ( 4.000000000000001776, 27.15624999877097423, 11.30940107675849760 ) ) ;
#7107 = VECTOR ( 'NONE', #13209, 1000.000000000000000 ) ;
#7108 = CARTESIAN_POINT ( 'NONE',  ( -22.67092431280609688, -21.28941499438201745, -6.500000000000000000 ) ) ;
#7109 = CARTESIAN_POINT ( 'NONE',  ( -27.10000000000000142, 0.000000000000000000, 1.000000000000000000 ) ) ;
#7110 = CARTESIAN_POINT ( 'NONE',  ( 20.40451381974352074, 17.74831644178408041, 12.25316411605952283 ) ) ;
#7111 = CIRCLE ( 'NONE', #4171, 0.5000000000000003331 ) ;
#7112 = CARTESIAN_POINT ( 'NONE',  ( 0.000000000000000000, 0.000000000000000000, 17.69999999999999929 ) ) ;
#7113 = CIRCLE ( 'NONE', #23815, 4.000000000000000000 ) ;
#7114 = EDGE_CURVE ( 'NONE', #18048, #1796, #11758, .T. ) ;
#7115 = CARTESIAN_POINT ( 'NONE',  ( 4.000000000000003553, 25.93750000000000000, 6.690598923241489970 ) ) ;
#7117 = EDGE_CURVE ( 'NONE', #22503, #12726, #5267, .T. ) ;
#7116 = AXIS2_PLACEMENT_3D ( 'NONE', #21013, #25194, #21130 ) ;
#7118 = CARTESIAN_POINT ( 'NONE',  ( 21.46744746577824969, 16.15505270985943298, 8.999999999999992895 ) ) ;
#7119 = CARTESIAN_POINT ( 'NONE',  ( 19.18911027444997686, 19.18911027444989870, 12.99999999999999112 ) ) ;
#7120 = ORIENTED_EDGE ( 'NONE', *, *, #18264, .F. ) ;
#7121 = CARTESIAN_POINT ( 'NONE',  ( 2.000000000000003553, 27.71874999877097778, 5.535898384862238508 ) ) ;
#7122 = EDGE_CURVE ( 'NONE', #14017, #21478, #6400, .T. ) ;
#7123 = CARTESIAN_POINT ( 'NONE',  ( -3.735045420075836212E-15, -26.60312499938547859, 4.662447845253954171 ) ) ;
#7124 = CIRCLE ( 'NONE', #21738, 4.000000000000000000 ) ;
#7125 = CARTESIAN_POINT ( 'NONE',  ( -1.878215178124995832, 26.75312499938548783, 5.746835883940462963 ) ) ;
#7126 = FACE_OUTER_BOUND ( 'NONE', #19823, .T. ) ;
#7128 = ORIENTED_EDGE ( 'NONE', *, *, #15842, .T. ) ;
#7127 = CARTESIAN_POINT ( 'NONE',  ( -3.756430356249997882, 29.04062499938548569, 6.831223922626973533 ) ) ;
#7129 = ORIENTED_EDGE ( 'NONE', *, *, #2128, .T. ) ;
#7130 = FACE_OUTER_BOUND ( 'NONE', #17510, .T. ) ;
#7131 = PRESENTATION_LAYER_ASSIGNMENT (  '', '', ( #23407 ) ) ;
#7132 = AXIS2_PLACEMENT_3D ( 'NONE', #25672, #4074, #12047 ) ;
#7133 = CARTESIAN_POINT ( 'NONE',  ( 4.000000000000003553, 26.33124999877097139, 6.690598923241489970 ) ) ;
#7134 = VERTEX_POINT ( 'NONE', #7617 ) ;
#7135 = CARTESIAN_POINT ( 'NONE',  ( 3.756430356249997438, -29.11562499938548498, 11.16877607737301048 ) ) ;
#7136 = LINE ( 'NONE', #24658, #14717 ) ;
#7137 = CARTESIAN_POINT ( 'NONE',  ( -3.756430356249994773, 25.81562499938548783, 8.999999999999992895 ) ) ;
#7138 = CIRCLE ( 'NONE', #17174, 0.5000000000000005551 ) ;
#7139 = CARTESIAN_POINT ( 'NONE',  ( -17.87326343783962201, -25.45105997952905597, 1.000000000000000000 ) ) ;
#7140 = CARTESIAN_POINT ( 'NONE',  ( 1.878215178125001605, 28.66562499938549280, 12.25316411605952283 ) ) ;
#7141 = EDGE_CURVE ( 'NONE', #1926, #21566, #15603, .T. ) ;
#7142 = CYLINDRICAL_SURFACE ( 'NONE', #11285, 0.5000000000000004441 ) ;
#7143 = DIRECTION ( 'NONE',  ( 0.3681245526846875782, 0.9297764858882475725, 0.000000000000000000 ) ) ;
#7144 = AXIS2_PLACEMENT_3D ( 'NONE', #12127, #20103, #10166 ) ;
#7145 = ADVANCED_FACE ( 'NONE', ( #17155 ), #21194, .F. ) ;
#7146 = CIRCLE ( 'NONE', #13012, 2.899999999999999911 ) ;
#7147 = CYLINDRICAL_SURFACE ( 'NONE', #5066, 31.10000000000000142 ) ;
#7148 = CARTESIAN_POINT ( 'NONE',  ( -1.878215178124995832, 27.09062499938548640, 5.746835883940462963 ) ) ;
#7149 = LINE ( 'NONE', #15139, #10368 ) ;
#7150 = CARTESIAN_POINT ( 'NONE',  ( 21.59775651299582222, 18.94155913503637478, 12.25316411605952283 ) ) ;
#7151 = CARTESIAN_POINT ( 'NONE',  ( 15.99595368409253915, 21.30834844001121553, 8.999999999999992895 ) ) ;
#7152 = CARTESIAN_POINT ( 'NONE',  ( 18.59690834520624136, 21.42533546995235838, 5.535898384862237620 ) ) ;
#7153 = CARTESIAN_POINT ( 'NONE',  ( -3.756430356249995661, 28.02812499938548640, 6.831223922626973533 ) ) ;
#7154 = DIRECTION ( 'NONE',  ( 0.000000000000000000, -0.000000000000000000, 1.000000000000000000 ) ) ;
#7155 = CARTESIAN_POINT ( 'NONE',  ( 15.91640417120904871, 21.22879892712773042, 8.999999999999992895 ) ) ;
#7156 = CARTESIAN_POINT ( 'NONE',  ( 22.28712185865447637, 19.45869473390820659, 5.535898384862238508 ) ) ;
#7157 = ORIENTED_EDGE ( 'NONE', *, *, #23697, .T. ) ;
#7158 = CARTESIAN_POINT ( 'NONE',  ( -27.10000000000000497, 0.6000000000000000888, 19.00000000000000000 ) ) ;
#7159 = CARTESIAN_POINT ( 'NONE',  ( -3.999999999999996003, 27.38124999877096855, 6.690598923241487306 ) ) ;
#7160 = CARTESIAN_POINT ( 'NONE',  ( -3.756430356250002323, -28.25312499938548427, 11.16877607737301226 ) ) ;
#7162 = VERTEX_POINT ( 'NONE', #16773 ) ;
#7161 = CARTESIAN_POINT ( 'NONE',  ( 5.335677986744788548, 30.63887302793246548, 1.000000000000000000 ) ) ;
#7163 = CARTESIAN_POINT ( 'NONE',  ( 1.878215178125000939, 26.52812499938548285, 12.25316411605952283 ) ) ;
#7164 = ADVANCED_FACE ( 'NONE', ( #20951 ), #24871, .F. ) ;
#7165 = AXIS2_PLACEMENT_3D ( 'NONE', #7108, #23071, #5156 ) ;
#7166 = ORIENTED_EDGE ( 'NONE', *, *, #362, .T. ) ;
#7167 = CARTESIAN_POINT ( 'NONE',  ( -2.672651547586948120E-15, -28.62812499938548783, 13.33755215474602984 ) ) ;
#7168 = ORIENTED_EDGE ( 'NONE', *, *, #14772, .T. ) ;
#7169 = PRODUCT ( 'casing', 'casing', '', ( #7276 ) ) ;
#7170 = VERTEX_POINT ( 'NONE', #16906 ) ;
#7171 = CARTESIAN_POINT ( 'NONE',  ( 20.46600609040033447, 21.93646478979743719, 12.87134967428165666 ) ) ;
#7172 = VECTOR ( 'NONE', #22696, 1000.000000000000000 ) ;
#7173 = CARTESIAN_POINT ( 'NONE',  ( 3.756430356250002323, 28.44062499938549138, 6.831223922626973533 ) ) ;
#7174 = AXIS2_PLACEMENT_3D ( 'NONE', #13799, #5685, #1781 ) ;
#7175 = DIRECTION ( 'NONE',  ( 1.000000000000000000, 0.000000000000000000, 0.000000000000000000 ) ) ;
#7176 = AXIS2_PLACEMENT_3D ( 'NONE', #1783, #18243, #4634 ) ;
#7177 = CARTESIAN_POINT ( 'NONE',  ( 3.756430356250002323, -11.16877607737301226, 3.365624999385485872 ) ) ;
#7178 = CARTESIAN_POINT ( 'NONE',  ( -8.831537335106614961E-15, -27.53124999877097068, 12.99999999999999112 ) ) ;
#7179 = CARTESIAN_POINT ( 'NONE',  ( 4.000000000000002665, 28.56249999999999645, 11.30940107675849760 ) ) ;
#7180 = CIRCLE ( 'NONE', #5094, 1.500000000000000222 ) ;
#7181 = DIRECTION ( 'NONE',  ( -0.000000000000000000, 0.000000000000000000, 1.000000000000000000 ) ) ;
#7182 = CARTESIAN_POINT ( 'NONE',  ( 3.756430356250002323, 28.70312499938548356, 11.16877607737301403 ) ) ;
#7183 = CARTESIAN_POINT ( 'NONE',  ( 16.90427148687188819, 22.56112573636419683, 11.30940107675849404 ) ) ;
#7184 = DIRECTION ( 'NONE',  ( -0.000000000000000000, 0.000000000000000000, -1.000000000000000000 ) ) ;
#7185 = DIRECTION ( 'NONE',  ( 0.8660254037844397068, -0.4999999999999983347, 0.000000000000000000 ) ) ;
#7186 = FACE_OUTER_BOUND ( 'NONE', #6941, .T. ) ;
#7187 = CARTESIAN_POINT ( 'NONE',  ( 1.878215178124998497, -29.15312499938548640, 12.25316411605951927 ) ) ;
#7188 = VECTOR ( 'NONE', #8743, 1000.000000000000000 ) ;
#7189 = CARTESIAN_POINT ( 'NONE',  ( 3.756430356250003655, 25.70312499938548356, 8.999999999999992895 ) ) ;
#7190 = ADVANCED_FACE ( 'NONE', ( #7075 ), #225, .F. ) ;
#7191 = AXIS2_PLACEMENT_3D ( 'NONE', #12812, #16999, #24963 ) ;
#7192 = DIRECTION ( 'NONE',  ( 0.000000000000000000, 0.000000000000000000, 1.000000000000000000 ) ) ;
#7193 = DIRECTION ( 'NONE',  ( -0.9048270524660170233, 0.4257792915650782661, 0.000000000000000000 ) ) ;
#7194 = DIRECTION ( 'NONE',  ( 0.000000000000000000, -0.000000000000000000, 1.000000000000000000 ) ) ;
#7195 = ORIENTED_EDGE ( 'NONE', *, *, #10760, .T. ) ;
#7196 = AXIS2_PLACEMENT_3D ( 'NONE', #1243, #17216, #23097 ) ;
#7197 = CARTESIAN_POINT ( 'NONE',  ( 31.03863125411925239, 1.952785157361540236, -6.500000000000000000 ) ) ;
#7199 = ORIENTED_EDGE ( 'NONE', *, *, #20821, .T. ) ;
#7198 = CARTESIAN_POINT ( 'NONE',  ( 21.05852382634284936, 21.05852382634277831, 12.99999999999999289 ) ) ;
#7200 = AXIS2_PLACEMENT_3D ( 'NONE', #4408, #6241, #23768 ) ;
#7201 = ORIENTED_EDGE ( 'NONE', *, *, #2824, .T. ) ;
#7202 = ORIENTED_EDGE ( 'NONE', *, *, #25667, .F. ) ;
#7203 = ORIENTED_EDGE ( 'NONE', *, *, #7433, .T. ) ;
#7204 = VERTEX_POINT ( 'NONE', #19678 ) ;
#7205 = CARTESIAN_POINT ( 'NONE',  ( 0.5000000000000000000, 0.000000000000000000, 20.00000000000000000 ) ) ;
#7206 = CARTESIAN_POINT ( 'NONE',  ( -3.469446951953614189E-15, -30.00000000000000355, 8.999999999999992895 ) ) ;
#7207 = VECTOR ( 'NONE', #12959, 1000.000000000000000 ) ;
#7208 = DIRECTION ( 'NONE',  ( 1.000000000000000000, 0.000000000000000000, 0.000000000000000000 ) ) ;
#7209 = CIRCLE ( 'NONE', #3448, 31.10000000000000142 ) ;
#7210 = CARTESIAN_POINT ( 'NONE',  ( -3.756430356249995661, -6.831223922626973533, 0.3281249993854827851 ) ) ;
#7211 = CARTESIAN_POINT ( 'NONE',  ( 2.620986760973688460E-15, -13.61880215351699874, 1.631249998770966991 ) ) ;
#7212 = CARTESIAN_POINT ( 'NONE',  ( 21.27955846146187113, 18.62336108350243080, 12.25316411605952283 ) ) ;
#7213 = CARTESIAN_POINT ( 'NONE',  ( 2.672651547586948120E-15, 26.49062499938548143, 13.33755215474602984 ) ) ;
#7214 = CYLINDRICAL_SURFACE ( 'NONE', #25483, 31.10000000000000142 ) ;
#7215 = FACE_OUTER_BOUND ( 'NONE', #18703, .T. ) ;
#7216 = CARTESIAN_POINT ( 'NONE',  ( -3.756430356249997882, -11.16877607737301226, 3.553124999385482763 ) ) ;
#7217 = CYLINDRICAL_SURFACE ( 'NONE', #22980, 0.5000000000000004441 ) ;
#7218 = CARTESIAN_POINT ( 'NONE',  ( -26.00000000000000711, 0.000000000000000000, 19.50000000000000000 ) ) ;
#7219 = DIRECTION ( 'NONE',  ( 1.000000000000000000, 0.000000000000000000, 0.000000000000000000 ) ) ;
#7220 = DIRECTION ( 'NONE',  ( 0.000000000000000000, -0.000000000000000000, 1.000000000000000000 ) ) ;
#7221 = CARTESIAN_POINT ( 'NONE',  ( 3.752267015613588906E-15, -4.381197846482986158, 0.5062499987709696558 ) ) ;
#7222 = CIRCLE ( 'NONE', #15164, 0.5000000000000011102 ) ;
#7223 = ADVANCED_FACE ( 'NONE', ( #15894 ), #3717, .T. ) ;
#7224 = CARTESIAN_POINT ( 'NONE',  ( -3.834746474454188013E-15, -25.56250000000000000, 4.999999999999992006 ) ) ;
#7225 = ORIENTED_EDGE ( 'NONE', *, *, #24143, .F. ) ;
#7226 = DIRECTION ( 'NONE',  ( 0.000000000000000000, 0.000000000000000000, 1.000000000000000000 ) ) ;
#7227 = ORIENTED_EDGE ( 'NONE', *, *, #2985, .F. ) ;
#7228 = AXIS2_PLACEMENT_3D ( 'NONE', #17548, #19875, #1975 ) ;
#7229 = EDGE_CURVE ( 'NONE', #17829, #990, #10129, .T. ) ;
#7230 = ORIENTED_EDGE ( 'NONE', *, *, #22294, .T. ) ;
#7231 = CARTESIAN_POINT ( 'NONE',  ( -3.878215178125003604, -29.82343749907822783, 8.999999999999992895 ) ) ;
#7232 = ORIENTED_EDGE ( 'NONE', *, *, #6314, .T. ) ;
#7233 = DIRECTION ( 'NONE',  ( 1.000000000000000000, 0.000000000000000000, 0.000000000000000000 ) ) ;
#7234 = EDGE_CURVE ( 'NONE', #10411, #25139, #6075, .T. ) ;
#7235 = ORIENTED_EDGE ( 'NONE', *, *, #25271, .T. ) ;
#7236 = CYLINDRICAL_SURFACE ( 'NONE', #79, 0.5000000000000002220 ) ;
#7237 = ORIENTED_EDGE ( 'NONE', *, *, #3425, .T. ) ;
#7238 = EDGE_CURVE ( 'NONE', #21069, #25296, #3009, .T. ) ;
#7239 = LINE ( 'NONE', #15088, #20162 ) ;
#7240 = CARTESIAN_POINT ( 'NONE',  ( -1.999999999999995781, 27.40000000000000213, 5.535898384862237620 ) ) ;
#7241 = CIRCLE ( 'NONE', #22716, 0.4999999999999992784 ) ;
#7242 = CARTESIAN_POINT ( 'NONE',  ( 31.09598070739550479, -0.4999838450259578293, 1.000000000000000000 ) ) ;
#7243 = CARTESIAN_POINT ( 'NONE',  ( 4.648177544792955347E-16, 25.78750000000000497, 12.99999999999999289 ) ) ;
#7244 = CARTESIAN_POINT ( 'NONE',  ( 21.46744746577824969, 16.15505270985943298, 8.999999999999992895 ) ) ;
#7245 =( BOUNDED_CURVE ( )  B_SPLINE_CURVE ( 2, ( #25413, #3972, #25682, #13781, #21759, #11820, #19792, #16013, #11937 ),
 .UNSPECIFIED., .F., .F. ) 
 B_SPLINE_CURVE_WITH_KNOTS ( ( 3, 2, 2, 2, 3 ),
 ( 0.1250000000000000000, 0.1333333333333333315, 0.1499999999999999944, 0.1666666666666666574, 0.1749999999999999889 ),
 .UNSPECIFIED. ) 
 CURVE ( )  GEOMETRIC_REPRESENTATION_ITEM ( )  RATIONAL_B_SPLINE_CURVE ( ( 0.9330127018922194093, 0.9330127018922194093, 1.000000000000000000, 0.8660254037844387076, 1.000000000000000000, 0.8660254037844387076, 1.000000000000000000, 0.9330127018922194093, 0.9330127018922194093 ) ) 
 REPRESENTATION_ITEM ( '' )  );
#7246 = CARTESIAN_POINT ( 'NONE',  ( -31.06601413805600842, 1.453535542772947942, 1.000000000000000000 ) ) ;
#7247 = CARTESIAN_POINT ( 'NONE',  ( 3.756430356250002323, 29.60312499938548569, 11.16877607737301226 ) ) ;
#7248 =( BOUNDED_CURVE ( )  B_SPLINE_CURVE ( 2, ( #16971, #1266, #15003, #9105, #17095, #25070, #7156, #23115, #11188 ),
 .UNSPECIFIED., .F., .F. ) 
 B_SPLINE_CURVE_WITH_KNOTS ( ( 3, 2, 2, 2, 3 ),
 ( 0.8750000000000000000, 0.8833333333333333037, 0.9000000000000000222, 0.9166666666666666297, 0.9249999999999999334 ),
 .UNSPECIFIED. ) 
 CURVE ( )  GEOMETRIC_REPRESENTATION_ITEM ( )  RATIONAL_B_SPLINE_CURVE ( ( 0.9330127018922194093, 0.9330127018922194093, 1.000000000000000000, 0.8660254037844387076, 1.000000000000000000, 0.8660254037844387076, 1.000000000000000000, 0.9330127018922198534, 0.9330127018922194093 ) ) 
 REPRESENTATION_ITEM ( '' )  );
#7249 = CARTESIAN_POINT ( 'NONE',  ( 21.81216202160669226, 16.49976726568787200, 6.831223922626973533 ) ) ;
#7250 = DIRECTION ( 'NONE',  ( 1.000000000000000000, 0.000000000000000000, 0.000000000000000000 ) ) ;
#7251 = EDGE_LOOP ( 'NONE', ( #7677, #16236, #16443, #1863 ) ) ;
#7252 = ORIENTED_EDGE ( 'NONE', *, *, #4704, .F. ) ;
#7253 = CARTESIAN_POINT ( 'NONE',  ( -1.999999999999994893, 27.79374999877096997, 5.535898384862237620 ) ) ;
#7254 = AXIS2_PLACEMENT_3D ( 'NONE', #11102, #9019, #15420 ) ;
#7255 = CARTESIAN_POINT ( 'NONE',  ( -3.756430356250002323, -28.70312499938548356, 11.16877607737301403 ) ) ;
#7256 = MECHANICAL_DESIGN_GEOMETRIC_PRESENTATION_REPRESENTATION (  '', ( #587 ), #17700 ) ;
#7257 = ORIENTED_EDGE ( 'NONE', *, *, #23882, .F. ) ;
#7258 = LINE ( 'NONE', #11039, #9168 ) ;
#7259 = CARTESIAN_POINT ( 'NONE',  ( 2.672651547586948120E-15, 27.39062499938548356, 13.33755215474602984 ) ) ;
#7260 = DIRECTION ( 'NONE',  ( 0.000000000000000000, -0.7071067811865503483, -0.7071067811865446862 ) ) ;
#7261 = ORIENTED_EDGE ( 'NONE', *, *, #5304, .T. ) ;
#7262 = ADVANCED_FACE ( 'NONE', ( #16152 ), #3715, .F. ) ;
#7263 = ORIENTED_EDGE ( 'NONE', *, *, #7770, .T. ) ;
#7264 = DIRECTION ( 'NONE',  ( -0.000000000000000000, -0.000000000000000000, 1.000000000000000000 ) ) ;
#7265 = DIRECTION ( 'NONE',  ( 1.000000000000000000, 0.000000000000000000, 0.000000000000000000 ) ) ;
#7266 = VERTEX_POINT ( 'NONE', #24363 ) ;
#7267 = EDGE_CURVE ( 'NONE', #6707, #7998, #22788, .T. ) ;
#7268 = CARTESIAN_POINT ( 'NONE',  ( -3.756430356250003655, -29.30312499938548498, 8.999999999999992895 ) ) ;
#7269 = CARTESIAN_POINT ( 'NONE',  ( 1.859271017917182139E-15, 25.78750000000000142, 12.99999999999999289 ) ) ;
#7270 = DIRECTION ( 'NONE',  ( -0.5877852522924775780, -0.8090169943749443426, 0.000000000000000000 ) ) ;
#7271 = EDGE_CURVE ( 'NONE', #21566, #5410, #5103, .T. ) ;
#7272 = MECHANICAL_DESIGN_GEOMETRIC_PRESENTATION_REPRESENTATION (  '', ( #22295 ), #10601 ) ;
#7273 = CARTESIAN_POINT ( 'NONE',  ( 22.38876845931909187, 16.73191420982663757, 11.30940107675849760 ) ) ;
#7274 = CARTESIAN_POINT ( 'NONE',  ( -3.756430356250000546, 28.55312499938549564, 11.16877607737301226 ) ) ;
#7275 = CARTESIAN_POINT ( 'NONE',  ( 0.000000000000000000, 0.000000000000000000, 15.00000000000000178 ) ) ;
#7276 = PRODUCT_CONTEXT ( 'NONE', #599, 'mechanical' ) ;
#7277 = DIRECTION ( 'NONE',  ( 0.000000000000000000, -0.000000000000000000, -1.000000000000000000 ) ) ;
#7278 = CARTESIAN_POINT ( 'NONE',  ( -3.959305671612554781E-15, -30.00000000000000355, 12.99999999999999289 ) ) ;
#7279 = CARTESIAN_POINT ( 'NONE',  ( 3.756430356250003211, 26.07812499938548356, 6.831223922626973533 ) ) ;
#7280 = CARTESIAN_POINT ( 'NONE',  ( -3.999999999999996447, 27.00624999877097565, 11.30940107675849404 ) ) ;
#7281 = CARTESIAN_POINT ( 'NONE',  ( 20.08404229395466700, 20.08404229395459240, 4.662447845253954171 ) ) ;
#7282 = CARTESIAN_POINT ( 'NONE',  ( 15.96943717979804056, 21.28183193571671694, 6.831223922626973533 ) ) ;
#7283 = CARTESIAN_POINT ( 'NONE',  ( 16.26787538380399312, 21.92472963329630531, 11.30940107675849404 ) ) ;
#7284 = CARTESIAN_POINT ( 'NONE',  ( 3.735045420075836212E-15, 27.50312499938548783, 4.662447845253954171 ) ) ;
#7285 = FACE_OUTER_BOUND ( 'NONE', #22422, .T. ) ;
#7286 = PRODUCT_DEFINITION_FORMATION_WITH_SPECIFIED_SOURCE ( 'ANY', '', #12142, .NOT_KNOWN. ) ;
#7287 = CARTESIAN_POINT ( 'NONE',  ( 21.38562447863985483, 18.72942710068040739, 5.746835883940462963 ) ) ;
#7288 = DIRECTION ( 'NONE',  ( 0.9297764858882561212, 0.3681245526846659843, 0.000000000000000000 ) ) ;
#7289 = ORIENTED_EDGE ( 'NONE', *, *, #5402, .T. ) ;
#7290 = CARTESIAN_POINT ( 'NONE',  ( 4.000000000000003553, 25.39374999877096784, 8.999999999999992895 ) ) ;
#7291 = CARTESIAN_POINT ( 'NONE',  ( 2.672651547586948120E-15, 26.49062499938548143, 13.33755215474602984 ) ) ;
#7292 = CARTESIAN_POINT ( 'NONE',  ( -3.735045420075836212E-15, -27.95312499938548001, 4.662447845253954171 ) ) ;
#7294 = ORIENTED_EDGE ( 'NONE', *, *, #54, .F. ) ;
#7293 = DIRECTION ( 'NONE',  ( 0.000000000000000000, 0.000000000000000000, 1.000000000000000000 ) ) ;
#7295 = CARTESIAN_POINT ( 'NONE',  ( -3.756430356249996105, 25.44062499938548427, 6.831223922626973533 ) ) ;
#7296 = VERTEX_POINT ( 'NONE', #14543 ) ;
#7297 = CARTESIAN_POINT ( 'NONE',  ( -3.756430356250004099, -27.87812499938548427, 6.831223922626973533 ) ) ;
#7298 = ORIENTED_EDGE ( 'NONE', *, *, #6426, .F. ) ;
#7299 = ORIENTED_EDGE ( 'NONE', *, *, #21623, .T. ) ;
#7300 = CARTESIAN_POINT ( 'NONE',  ( 18.61651080183891338, 23.52545784775749382, 6.994934987683498306 ) ) ;
#7301 = CARTESIAN_POINT ( 'NONE',  ( -1.878215178124999829, 28.70312499938548711, 12.25316411605951927 ) ) ;
#7302 = EDGE_CURVE ( 'NONE', #6155, #12209, #2571, .T. ) ;
#7303 = AXIS2_PLACEMENT_3D ( 'NONE', #17339, #19526, #25305 ) ;
#7304 = CARTESIAN_POINT ( 'NONE',  ( 3.756430356250003655, -8.999999999999992895, 1.490624999385483429 ) ) ;
#7305 = CARTESIAN_POINT ( 'NONE',  ( 3.756430356250003655, -8.999999999999992895, 3.853124999385483473 ) ) ;
#7306 = CARTESIAN_POINT ( 'NONE',  ( 3.999999999999996447, -27.41874999877096641, 8.999999999999992895 ) ) ;
#7307 = DIRECTION ( 'NONE',  ( -0.6374239897486919659, -0.7705132427757873659, 0.000000000000000000 ) ) ;
#7308 = CARTESIAN_POINT ( 'NONE',  ( 30.24338421796784004, 7.248980000274092284, -2.750000000000000000 ) ) ;
#7309 = PRODUCT_DEFINITION_CONTEXT ( 'detailed design', #2921, 'design' ) ;
#7310 = CARTESIAN_POINT ( 'NONE',  ( -3.137519842735244810E-15, 26.46249999999999858, 4.999999999999991118 ) ) ;
#7311 = LINE ( 'NONE', #25098, #20393 ) ;
#7312 = PLANE ( 'NONE',  #22650 ) ;
#7313 = CARTESIAN_POINT ( 'NONE',  ( -2.000000000000003997, -27.71874999877097068, 5.535898384862238508 ) ) ;
#7314 = CARTESIAN_POINT ( 'NONE',  ( -2.672651547586948120E-15, -28.74062499938548498, 13.33755215474602984 ) ) ;
#7315 = DIRECTION ( 'NONE',  ( -0.000000000000000000, -1.000000000000000000, -0.000000000000000000 ) ) ;
#7316 = PLANE ( 'NONE',  #11234 ) ;
#7317 = DIRECTION ( 'NONE',  ( -0.000000000000000000, -1.000000000000000000, -0.000000000000000000 ) ) ;
#7318 = ORIENTED_EDGE ( 'NONE', *, *, #10618, .T. ) ;
#7319 = CARTESIAN_POINT ( 'NONE',  ( -4.000000000000003553, -25.00000000000000000, 8.999999999999992895 ) ) ;
#7320 = CARTESIAN_POINT ( 'NONE',  ( 3.469446951953614189E-15, 38.49999999999999289, 8.999999999999992895 ) ) ;
#7322 = ORIENTED_EDGE ( 'NONE', *, *, #21921, .T. ) ;
#7321 = CARTESIAN_POINT ( 'NONE',  ( 18.68225429291714690, -24.86329371854781201, 1.000000000000000000 ) ) ;
#7323 = VERTEX_POINT ( 'NONE', #12322 ) ;
#7324 = ORIENTED_EDGE ( 'NONE', *, *, #532, .T. ) ;
#7325 = ORIENTED_EDGE ( 'NONE', *, *, #14470, .F. ) ;
#7326 = ORIENTED_EDGE ( 'NONE', *, *, #6680, .T. ) ;
#7327 = EDGE_CURVE ( 'NONE', #7090, #19352, #1329, .T. ) ;
#7328 = DIRECTION ( 'NONE',  ( 0.000000000000000000, -1.000000000000000000, 0.000000000000000000 ) ) ;
#7329 = CARTESIAN_POINT ( 'NONE',  ( 0.000000000000000000, 0.000000000000000000, 19.59999999999999787 ) ) ;
#7330 = CARTESIAN_POINT ( 'NONE',  ( 4.006172263299091013E-15, 25.25312499938549138, 4.662447845253954171 ) ) ;
#7331 = EDGE_CURVE ( 'NONE', #14404, #11374, #8437, .T. ) ;
#7332 = CARTESIAN_POINT ( 'NONE',  ( 3.735045420075836212E-15, -4.662447845253954171, 3.965624999385486404 ) ) ;
#7333 = CARTESIAN_POINT ( 'NONE',  ( -1.999999999999998224, -12.46410161513774639, 2.043749998770966414 ) ) ;
#7334 = LINE ( 'NONE', #23547, #20612 ) ;
#7335 = CARTESIAN_POINT ( 'NONE',  ( 3.756430356250002323, 25.66562499938548569, 11.16877607737301226 ) ) ;
#7336 = EDGE_CURVE ( 'NONE', #22817, #5616, #10926, .T. ) ;
#7337 = DIRECTION ( 'NONE',  ( 0.000000000000000000, 0.000000000000000000, 1.000000000000000000 ) ) ;
#7338 = LINE ( 'NONE', #15447, #10511 ) ;
#7339 = CARTESIAN_POINT ( 'NONE',  ( 2.672651547586948120E-15, -13.33755215474602984, 3.628124999385485161 ) ) ;
#7340 = CIRCLE ( 'NONE', #12341, 0.4999999999999993339 ) ;
#7341 = DIRECTION ( 'NONE',  ( 0.000000000000000000, 0.000000000000000000, 1.000000000000000000 ) ) ;
#7342 = CARTESIAN_POINT ( 'NONE',  ( -3.469446951953614189E-15, -30.00000000000000355, 4.999999999999992006 ) ) ;
#7343 = CARTESIAN_POINT ( 'NONE',  ( 3.959305671612554781E-15, 35.50000000000000711, 12.99999999999999289 ) ) ;
#7344 = CARTESIAN_POINT ( 'NONE',  ( -2.000000000000000888, -26.21874999877096712, 12.46410161513774817 ) ) ;
#7345 = CARTESIAN_POINT ( 'NONE',  ( 2.672651547586948120E-15, -13.33755215474603162, 3.740624999385483651 ) ) ;
#7346 = DIRECTION ( 'NONE',  ( -0.000000000000000000, -0.000000000000000000, -1.000000000000000000 ) ) ;
#7347 = DIRECTION ( 'NONE',  ( 0.000000000000000000, 0.000000000000000000, 1.000000000000000000 ) ) ;
#7348 = DIRECTION ( 'NONE',  ( 0.000000000000000000, 0.000000000000000000, 1.000000000000000000 ) ) ;
#7349 = EDGE_LOOP ( 'NONE', ( #4683, #15048, #1416, #12309 ) ) ;
#7350 = DIRECTION ( 'NONE',  ( 0.9980267284282714479, -0.06279051952931540004, 0.000000000000000000 ) ) ;
#7351 = VERTEX_POINT ( 'NONE', #16252 ) ;
#7352 = ORIENTED_EDGE ( 'NONE', *, *, #21065, .T. ) ;
#7353 = DIRECTION ( 'NONE',  ( 1.000000000000000000, 0.000000000000000000, 0.000000000000000000 ) ) ;
#7354 =( BOUNDED_CURVE ( )  B_SPLINE_CURVE ( 2, ( #18915, #19034, #1115, #7273, #17077, #25051, #1247, #9230, #21634 ),
 .UNSPECIFIED., .F., .F. ) 
 B_SPLINE_CURVE_WITH_KNOTS ( ( 3, 2, 2, 2, 3 ),
 ( 0.5750000000000000666, 0.5833333333333333703, 0.5999999999999999778, 0.6166666666666666963, 0.6250000000000000000 ),
 .UNSPECIFIED. ) 
 CURVE ( )  GEOMETRIC_REPRESENTATION_ITEM ( )  RATIONAL_B_SPLINE_CURVE ( ( 0.9330127018922194093, 0.9330127018922198534, 1.000000000000000000, 0.8660254037844387076, 1.000000000000000000, 0.8660254037844387076, 1.000000000000000000, 0.9330127018922194093, 0.9330127018922194093 ) ) 
 REPRESENTATION_ITEM ( '' )  );
#7355 = ORIENTED_EDGE ( 'NONE', *, *, #10213, .F. ) ;
#7356 = VECTOR ( 'NONE', #14320, 1000.000000000000000 ) ;
#7357 = CARTESIAN_POINT ( 'NONE',  ( 1.878215178124998497, -29.15312499938548640, 12.25316411605951927 ) ) ;
#7358 = ORIENTED_EDGE ( 'NONE', *, *, #2378, .T. ) ;
#7359 = CARTESIAN_POINT ( 'NONE',  ( -30.85476721088030061, -3.897863563849544466, -6.500000000000000000 ) ) ;
#7360 = VERTEX_POINT ( 'NONE', #14303 ) ;
#7361 = CARTESIAN_POINT ( 'NONE',  ( 2.000000000000003997, 26.87500000000000355, 5.535898384862238508 ) ) ;
#7362 = CARTESIAN_POINT ( 'NONE',  ( 12.78762572734037484, -28.34936733434209444, -6.500000000000000000 ) ) ;
#7363 = EDGE_CURVE ( 'NONE', #23296, #6393, #492, .T. ) ;
#7364 = CARTESIAN_POINT ( 'NONE',  ( -1.999999999999995781, 26.50000000000000355, 5.535898384862237620 ) ) ;
#7365 = DIRECTION ( 'NONE',  ( 1.000000000000000000, 0.000000000000000000, 0.000000000000000000 ) ) ;
#7366 = CARTESIAN_POINT ( 'NONE',  ( 20.16359180683815921, 20.16359180683807750, 4.662447845253954171 ) ) ;
#7367 = FACE_OUTER_BOUND ( 'NONE', #14655, .T. ) ;
#7368 = CARTESIAN_POINT ( 'NONE',  ( 2.000000000000003997, 25.97500000000000142, 5.535898384862238508 ) ) ;
#7369 = CARTESIAN_POINT ( 'NONE',  ( 16.95054783869437642, 22.26294259461305103, 8.999999999999992895 ) ) ;
#7370 = CARTESIAN_POINT ( 'NONE',  ( -4.000000000000003553, -25.19687499938548569, 8.999999999999992895 ) ) ;
#7371 = ORIENTED_EDGE ( 'NONE', *, *, #3301, .T. ) ;
#7372 = ORIENTED_EDGE ( 'NONE', *, *, #16182, .F. ) ;
#7373 = CARTESIAN_POINT ( 'NONE',  ( 4.000000000000003553, 28.54374999877097707, 8.999999999999992895 ) ) ;
#7374 = CARTESIAN_POINT ( 'NONE',  ( -3.756430356250003211, -28.77812499938548285, 6.831223922626973533 ) ) ;
#7375 = ORIENTED_EDGE ( 'NONE', *, *, #12297, .F. ) ;
#7376 = CYLINDRICAL_SURFACE ( 'NONE', #19185, 2.899999999999999911 ) ;
#7377 = CARTESIAN_POINT ( 'NONE',  ( 3.735045420075836212E-15, 26.71562499938548640, 4.662447845253954171 ) ) ;
#7378 = DIRECTION ( 'NONE',  ( 0.000000000000000000, 1.000000000000000000, 0.000000000000000000 ) ) ;
#7379 = ORIENTED_EDGE ( 'NONE', *, *, #3657, .T. ) ;
#7380 = ORIENTED_EDGE ( 'NONE', *, *, #15303, .T. ) ;
#7381 = DIRECTION ( 'NONE',  ( 0.000000000000000000, -1.000000000000000000, 0.000000000000000000 ) ) ;
#7382 = CARTESIAN_POINT ( 'NONE',  ( -3.878215178125003604, -25.07031249969274356, 8.999999999999992895 ) ) ;
#7383 = EDGE_LOOP ( 'NONE', ( #16892, #2588, #1981, #13973 ) ) ;
#7384 = EDGE_CURVE ( 'NONE', #18733, #20971, #20412, .T. ) ;
#7385 = DIRECTION ( 'NONE',  ( 0.000000000000000000, 0.000000000000000000, 1.000000000000000000 ) ) ;
#7386 = CYLINDRICAL_SURFACE ( 'NONE', #4696, 31.10000000000000142 ) ;
#7387 = CARTESIAN_POINT ( 'NONE',  ( 8.012344526598182026E-15, 27.05312499938548854, 4.662447845253954171 ) ) ;
#7388 = DIRECTION ( 'NONE',  ( -0.000000000000000000, -0.000000000000000000, 1.000000000000000000 ) ) ;
#7389 = CARTESIAN_POINT ( 'NONE',  ( -1.878215178124996498, 28.44062499938548783, 5.746835883940462963 ) ) ;
#7390 =( BOUNDED_CURVE ( )  B_SPLINE_CURVE ( 2, ( #2693, #14731, #22708, #4789, #12764, #860, #2813 ),
 .UNSPECIFIED., .F., .F. ) 
 B_SPLINE_CURVE_WITH_KNOTS ( ( 3, 2, 2, 3 ),
 ( 0.8499999999999998668, 0.8666666666666664742, 0.8833333333333330817, 0.8999999999999996891 ),
 .UNSPECIFIED. ) 
 CURVE ( )  GEOMETRIC_REPRESENTATION_ITEM ( )  RATIONAL_B_SPLINE_CURVE ( ( 1.000000000000000888, 0.8660254037844378194, 1.000000000000000000, 0.8660254037844387076, 1.000000000000000000, 0.8660254037844413721, 0.9999999999999973355 ) ) 
 REPRESENTATION_ITEM ( '' )  );
#7391 = ADVANCED_FACE ( 'NONE', ( #6689 ), #692, .F. ) ;
#7392 = EDGE_CURVE ( 'NONE', #8164, #19322, #436, .T. ) ;
#7393 = CARTESIAN_POINT ( 'NONE',  ( 19.43607991388988765, 24.27856662945500688, 1.000000000000000000 ) ) ;
#7394 = DIRECTION ( 'NONE',  ( 0.000000000000000000, -0.000000000000000000, 1.000000000000000000 ) ) ;
#7395 = CARTESIAN_POINT ( 'NONE',  ( -1.878215178124995832, 26.19062499938548427, 5.746835883940462963 ) ) ;
#7396 = DIRECTION ( 'NONE',  ( 1.000000000000000000, 0.000000000000000000, 0.000000000000000000 ) ) ;
#7397 = CARTESIAN_POINT ( 'NONE',  ( 23.00540471485899374, 17.69300995894016992, 6.831223922626973533 ) ) ;
#7398 = CARTESIAN_POINT ( 'NONE',  ( 22.71372316761954124, 17.40132841170072808, 11.16877607737301226 ) ) ;
#7399 = EDGE_CURVE ( 'NONE', #32, #16533, #11745, .T. ) ;
#7400 = CARTESIAN_POINT ( 'NONE',  ( 21.21320343559646915, 21.21320343559638744, 8.999999999999992895 ) ) ;
#7401 = CARTESIAN_POINT ( 'NONE',  ( -3.756430356249997882, 29.45312499938548356, 11.16877607737301226 ) ) ;
#7402 = CARTESIAN_POINT ( 'NONE',  ( -24.86329371854788661, -18.68225429291705098, -6.500000000000000000 ) ) ;
#7403 = CARTESIAN_POINT ( 'NONE',  ( 21.73261250872320005, 16.42021775280438689, 6.831223922626973533 ) ) ;
#7404 = DIRECTION ( 'NONE',  ( 0.000000000000000000, -1.000000000000000000, 0.000000000000000000 ) ) ;
#7405 = ORIENTED_EDGE ( 'NONE', *, *, #3606, .T. ) ;
#7406 = CARTESIAN_POINT ( 'NONE',  ( -1.999999999999998224, 26.14374999877096784, 12.46410161513774639 ) ) ;
#7407 = CARTESIAN_POINT ( 'NONE',  ( 3.756430356250003655, 26.60312499938548569, 8.999999999999992895 ) ) ;
#7408 = CARTESIAN_POINT ( 'NONE',  ( -1.878215178125000939, -29.56562499938548427, 12.25316411605952283 ) ) ;
#7410 = VERTEX_POINT ( 'NONE', #16637 ) ;
#7409 = CARTESIAN_POINT ( 'NONE',  ( -2.003086131649545506E-15, 26.04062499938549280, 13.33755215474603162 ) ) ;
#7411 = CARTESIAN_POINT ( 'NONE',  ( 3.959305671612554781E-15, 40.00000000000000000, 12.99999999999999289 ) ) ;
#7412 = VERTEX_POINT ( 'NONE', #16522 ) ;
#7413 = CARTESIAN_POINT ( 'NONE',  ( -3.756430356250003655, -28.74062499938548498, 8.999999999999992895 ) ) ;
#7414 = EDGE_LOOP ( 'NONE', ( #2205, #18139, #25306, #7583 ) ) ;
#7415 = ORIENTED_EDGE ( 'NONE', *, *, #2634, .T. ) ;
#7416 = CARTESIAN_POINT ( 'NONE',  ( 18.35963726379211991, 23.72622656523767759, 7.708599238039754553 ) ) ;
#7417 = CARTESIAN_POINT ( 'NONE',  ( 3.756430356250003211, 25.59062499938548285, 8.999999999999992895 ) ) ;
#7418 = CARTESIAN_POINT ( 'NONE',  ( 3.756430356250002323, -11.16877607737301403, 0.5531249993854806535 ) ) ;
#7419 = CIRCLE ( 'NONE', #7887, 2.899999999999999911 ) ;
#7420 = CARTESIAN_POINT ( 'NONE',  ( -3.756430356249997882, -11.16877607737301226, 4.565624999385485161 ) ) ;
#7421 = CARTESIAN_POINT ( 'NONE',  ( 1.999999999999995781, -27.34374999877097068, 5.535898384862237620 ) ) ;
#7422 = CARTESIAN_POINT ( 'NONE',  ( 1.071796769724495002, 26.89240381056767504, 4.999999999999989342 ) ) ;
#7423 = CARTESIAN_POINT ( 'NONE',  ( 5.827558883615830965, -30.54913349766226105, -6.500000000000000000 ) ) ;
#7424 = DIRECTION ( 'NONE',  ( 0.8763066800438640280, -0.4817536741017146018, 0.000000000000000000 ) ) ;
#7425 = CARTESIAN_POINT ( 'NONE',  ( -1.071796769724488563, 27.06115380933863435, 12.99999999999999289 ) ) ;
#7426 = CARTESIAN_POINT ( 'NONE',  ( -0.5000000000000001110, 10.00000000000000000, 15.00000000000000178 ) ) ;
#7427 = CARTESIAN_POINT ( 'NONE',  ( 18.35384038830430597, 18.35384038830423492, 4.381197846482986158 ) ) ;
#7428 = EDGE_CURVE ( 'NONE', #9493, #16293, #8790, .T. ) ;
#7429 = VERTEX_POINT ( 'NONE', #6562 ) ;
#7430 = CARTESIAN_POINT ( 'NONE',  ( -4.000000000000003553, -27.68124999877096926, 6.690598923241489970 ) ) ;
#7431 = CARTESIAN_POINT ( 'NONE',  ( -3.756430356250004099, -28.89062499938548356, 6.831223922626973533 ) ) ;
#7432 = DIRECTION ( 'NONE',  ( 0.000000000000000000, 0.000000000000000000, 1.000000000000000000 ) ) ;
#7433 = EDGE_CURVE ( 'NONE', #19275, #7768, #10613, .T. ) ;
#7434 = CARTESIAN_POINT ( 'NONE',  ( 23.64116323484232751, -20.20656826142281659, 1.000000000000000000 ) ) ;
#7435 = CARTESIAN_POINT ( 'NONE',  ( 14.54246377227358877, 27.49048467073853175, -2.750000000000000000 ) ) ;
#7436 = CARTESIAN_POINT ( 'NONE',  ( -4.000000000000001776, -28.56249999999999645, 11.30940107675849760 ) ) ;
#7437 = ORIENTED_EDGE ( 'NONE', *, *, #17040, .F. ) ;
#7438 = FACE_OUTER_BOUND ( 'NONE', #21120, .T. ) ;
#7439 = LINE ( 'NONE', #15427, #18375 ) ;
#7441 = ORIENTED_EDGE ( 'NONE', *, *, #4104, .T. ) ;
#7440 = DIRECTION ( 'NONE',  ( 1.000000000000000000, 0.000000000000000000, 0.000000000000000000 ) ) ;
#7442 = EDGE_CURVE ( 'NONE', #4853, #18321, #8656, .T. ) ;
#7443 = EDGE_LOOP ( 'NONE', ( #21989, #15425, #12232, #15814 ) ) ;
#7444 = EDGE_CURVE ( 'NONE', #2906, #18910, #18218, .T. ) ;
#7445 = AXIS2_PLACEMENT_3D ( 'NONE', #21719, #6027, #17545 ) ;
#7446 = ORIENTED_EDGE ( 'NONE', *, *, #344, .F. ) ;
#7447 = ORIENTED_EDGE ( 'NONE', *, *, #21042, .T. ) ;
#7448 = ORIENTED_EDGE ( 'NONE', *, *, #6935, .F. ) ;
#7449 = DIRECTION ( 'NONE',  ( 0.000000000000000000, 0.000000000000000000, 1.000000000000000000 ) ) ;
#7450 = CARTESIAN_POINT ( 'NONE',  ( -25.16042852506104666, -18.28012134629567598, -6.500000000000000000 ) ) ;
#7451 = EDGE_CURVE ( 'NONE', #17713, #12604, #10894, .T. ) ;
#7452 = DIRECTION ( 'NONE',  ( 1.000000000000000000, 0.000000000000000000, 0.000000000000000000 ) ) ;
#7453 = CARTESIAN_POINT ( 'NONE',  ( -3.756430356249996994, -8.999999999999992895, 3.515624999385482674 ) ) ;
#7454 = CARTESIAN_POINT ( 'NONE',  ( 4.000000000000001776, -11.30940107675849760, 2.156249998770968457 ) ) ;
#7455 = CARTESIAN_POINT ( 'NONE',  ( -3.756430356249997882, 27.31562499938548427, 11.16877607737301226 ) ) ;
#7456 = CARTESIAN_POINT ( 'NONE',  ( 0.000000000000000000, 0.000000000000000000, 1.000000000000000000 ) ) ;
#7457 = VECTOR ( 'NONE', #10038, 1000.000000000000000 ) ;
#7458 = CARTESIAN_POINT ( 'NONE',  ( -3.999999999999996447, -8.999999999999992895, 18.00000000000000000 ) ) ;
#7459 = CARTESIAN_POINT ( 'NONE',  ( 4.000000000000003553, -6.690598923241489970, 0.9375000000000004441 ) ) ;
#7460 = AXIS2_PLACEMENT_3D ( 'NONE', #23729, #22028, #8052 ) ;
#7461 = CARTESIAN_POINT ( 'NONE',  ( -7.734255490826573265, 30.12293631110053838, -6.500000000000000000 ) ) ;
#7462 = DIRECTION ( 'NONE',  ( -0.000000000000000000, -0.000000000000000000, 1.000000000000000000 ) ) ;
#7463 = DIRECTION ( 'NONE',  ( 0.000000000000000000, 0.000000000000000000, 1.000000000000000000 ) ) ;
#7464 = CARTESIAN_POINT ( 'NONE',  ( -2.000000000000003997, -25.91874999877096997, 5.535898384862238508 ) ) ;
#7465 = CARTESIAN_POINT ( 'NONE',  ( -1.878215178124995832, -5.746835883940462963, 3.553124999385485427 ) ) ;
#7467 = ADVANCED_FACE ( 'NONE', ( #13230 ), #22910, .T. ) ;
#7466 = AXIS2_PLACEMENT_3D ( 'NONE', #19026, #991, #23207 ) ;
#7468 = DIRECTION ( 'NONE',  ( 1.000000000000000000, 0.000000000000000000, 0.000000000000000000 ) ) ;
#7470 = DIRECTION ( 'NONE',  ( 0.000000000000000000, 0.000000000000000000, 1.000000000000000000 ) ) ;
#7469 = VECTOR ( 'NONE', #7347, 1000.000000000000000 ) ;
#7471 = CARTESIAN_POINT ( 'NONE',  ( -3.999999999999997335, 25.71249999999999503, 11.30940107675849404 ) ) ;
#7472 = VERTEX_POINT ( 'NONE', #4995 ) ;
#7473 = CARTESIAN_POINT ( 'NONE',  ( 31.00322564728514507, 2.451530025009026392, 1.000000000000000000 ) ) ;
#7474 = VERTEX_POINT ( 'NONE', #25378 ) ;
#7475 = ORIENTED_EDGE ( 'NONE', *, *, #19884, .F. ) ;
#7476 = FACE_OUTER_BOUND ( 'NONE', #25004, .T. ) ;
#7477 = ORIENTED_EDGE ( 'NONE', *, *, #22102, .F. ) ;
#7478 = CARTESIAN_POINT ( 'NONE',  ( 1.878215178124998497, -26.90312499938548285, 12.25316411605951927 ) ) ;
#7479 = ORIENTED_EDGE ( 'NONE', *, *, #19066, .T. ) ;
#7480 = DIRECTION ( 'NONE',  ( 1.000000000000000000, 0.000000000000000000, 0.000000000000000000 ) ) ;
#7481 = EDGE_CURVE ( 'NONE', #16527, #22953, #23868, .T. ) ;
#7482 = AXIS2_PLACEMENT_3D ( 'NONE', #8638, #16616, #4725 ) ;
#7483 = ORIENTED_EDGE ( 'NONE', *, *, #16907, .F. ) ;
#7484 = CARTESIAN_POINT ( 'NONE',  ( -3.999999999999996003, 28.33750000000000213, 6.690598923241487306 ) ) ;
#7485 = DIRECTION ( 'NONE',  ( 1.000000000000000000, 0.000000000000000000, 0.000000000000000000 ) ) ;
#7486 = AXIS2_PLACEMENT_3D ( 'NONE', #22762, #6663, #16495 ) ;
#7487 = CARTESIAN_POINT ( 'NONE',  ( 3.756430356250003655, -8.999999999999992895, 0.7031249993854835623 ) ) ;
#7488 = DIRECTION ( 'NONE',  ( 0.000000000000000000, 0.000000000000000000, 1.000000000000000000 ) ) ;
#7489 = CARTESIAN_POINT ( 'NONE',  ( 21.46517399152334704, 18.80897661356389605, 5.746835883940462963 ) ) ;
#7490 = DIRECTION ( 'NONE',  ( -0.000000000000000000, -1.000000000000000000, -0.000000000000000000 ) ) ;
#7491 = CARTESIAN_POINT ( 'NONE',  ( 4.000000000000003553, 25.00000000000000000, 8.999999999999992895 ) ) ;
#7492 = CARTESIAN_POINT ( 'NONE',  ( 18.89079960070236908, 18.89079960070229802, 4.662447845253954171 ) ) ;
#7493 = DIRECTION ( 'NONE',  ( 8.659560562354900811E-17, -0.7071067811865503483, 0.7071067811865446862 ) ) ;
#7494 = CIRCLE ( 'NONE', #16281, 31.10000000000000142 ) ;
#7495 = ORIENTED_EDGE ( 'NONE', *, *, #12221, .F. ) ;
#7496 = ORIENTED_EDGE ( 'NONE', *, *, #14702, .T. ) ;
#7497 = CARTESIAN_POINT ( 'NONE',  ( -3.999999999999999556, 27.90624999877097778, 11.30940107675849404 ) ) ;
#7499 = CARTESIAN_POINT ( 'NONE',  ( 4.000000000000003553, 28.18750000000000000, 6.690598923241489970 ) ) ;
#7498 = VECTOR ( 'NONE', #17256, 1000.000000000000000 ) ;
#7500 = ORIENTED_EDGE ( 'NONE', *, *, #9920, .T. ) ;
#7501 = CARTESIAN_POINT ( 'NONE',  ( 30.85476721088025442, -3.897863563849982782, -6.500000000000000000 ) ) ;
#7502 = CIRCLE ( 'NONE', #22118, 0.5000000000000005551 ) ;
#7503 = ADVANCED_FACE ( 'NONE', ( #17296 ), #16912, .F. ) ;
#7504 = CARTESIAN_POINT ( 'NONE',  ( 1.878215178125004048, 28.92812499938548854, 5.746835883940462963 ) ) ;
#7505 = CARTESIAN_POINT ( 'NONE',  ( 1.071796769724498999, 28.00134618820329635, 12.99999999999998757 ) ) ;
#7506 = VERTEX_POINT ( 'NONE', #12973 ) ;
#7507 = ORIENTED_EDGE ( 'NONE', *, *, #3335, .F. ) ;
#7508 = CARTESIAN_POINT ( 'NONE',  ( 0.000000000000000000, 0.000000000000000000, -6.500000000000000000 ) ) ;
#7509 = VECTOR ( 'NONE', #15840, 1000.000000000000000 ) ;
#7510 = EDGE_LOOP ( 'NONE', ( #9564, #14844, #17583, #10328, #2946, #5078, #10015, #14168 ) ) ;
#7511 = LINE ( 'NONE', #23601, #19349 ) ;
#7512 = CARTESIAN_POINT ( 'NONE',  ( -3.756430356249996994, 25.81562499938548427, 8.999999999999992895 ) ) ;
#7513 = CARTESIAN_POINT ( 'NONE',  ( 3.756430356250002323, 28.32812499938548356, 6.831223922626973533 ) ) ;
#7514 = AXIS2_PLACEMENT_3D ( 'NONE', #20688, #6687, #1071 ) ;
#7515 = CARTESIAN_POINT ( 'NONE',  ( 3.469446951953614189E-15, 35.50000000000000711, 4.999999999999992006 ) ) ;
#7516 = CARTESIAN_POINT ( 'NONE',  ( 4.000000000000005329, 26.80000000000000426, 8.999999999999992895 ) ) ;
#7517 = CARTESIAN_POINT ( 'NONE',  ( 3.735045420075836212E-15, 29.30312499938548498, 4.662447845253954171 ) ) ;
#7518 = CARTESIAN_POINT ( 'NONE',  ( 8.831537335106614961E-15, 27.13750000000000284, 12.99999999999999112 ) ) ;
#7519 = CARTESIAN_POINT ( 'NONE',  ( 3.469446951953614189E-15, 40.00000000000000000, 8.999999999999992895 ) ) ;
#7520 = CARTESIAN_POINT ( 'NONE',  ( 1.878215178125004048, 27.01562499938548711, 5.746835883940462963 ) ) ;
#7521 = VECTOR ( 'NONE', #3321, 1000.000000000000000 ) ;
#7522 = CARTESIAN_POINT ( 'NONE',  ( 3.878215178125003604, 29.82343749907823138, 8.999999999999992895 ) ) ;
#7524 = EDGE_CURVE ( 'NONE', #11405, #22637, #4247, .T. ) ;
#7523 = CARTESIAN_POINT ( 'NONE',  ( 22.12360341637413796, 16.46674916688168366, 6.690598923241489970 ) ) ;
#7525 = CARTESIAN_POINT ( 'NONE',  ( 18.96807563933094798, 21.62427301729024975, 12.25316411605951927 ) ) ;
#7526 = CARTESIAN_POINT ( 'NONE',  ( -30.85476721088030061, -3.897863563849544466, 1.000000000000000000 ) ) ;
#7527 = CARTESIAN_POINT ( 'NONE',  ( 3.834746474454188013E-15, 28.26249999999999929, 4.999999999999992006 ) ) ;
#7528 = CYLINDRICAL_SURFACE ( 'NONE', #800, 31.10000000000000142 ) ;
#7529 = AXIS2_PLACEMENT_3D ( 'NONE', #23356, #17863, #5580 ) ;
#7530 = EDGE_CURVE ( 'NONE', #15689, #22370, #23361, .T. ) ;
#7531 = CARTESIAN_POINT ( 'NONE',  ( 21.41441445718925962, 16.10201970127043936, 6.831223922626973533 ) ) ;
#7532 = CARTESIAN_POINT ( 'NONE',  ( 4.000000000000001776, 25.84374999877097423, 8.999999999999992895 ) ) ;
#7533 = VERTEX_POINT ( 'NONE', #13363 ) ;
#7534 = CARTESIAN_POINT ( 'NONE',  ( 19.99344423804966198, 17.16501711330340996, 12.46410161513774817 ) ) ;
#7535 = CARTESIAN_POINT ( 'NONE',  ( 1.999999999999995781, -26.50000000000000355, 5.535898384862237620 ) ) ;
#7537 = VERTEX_POINT ( 'NONE', #9047 ) ;
#7536 = LINE ( 'NONE', #17479, #1246 ) ;
#7538 = CARTESIAN_POINT ( 'NONE',  ( 1.878215178125004048, 27.12812499938548783, 5.746835883940462963 ) ) ;
#7539 = EDGE_CURVE ( 'NONE', #7580, #12699, #20115, .T. ) ;
#7540 = DIRECTION ( 'NONE',  ( 0.000000000000000000, -1.000000000000000000, 0.000000000000000000 ) ) ;
#7541 = CARTESIAN_POINT ( 'NONE',  ( -23.36965697125209473, 11.52193136556784481, 20.00001200000000168 ) ) ;
#7542 = DIRECTION ( 'NONE',  ( 0.000000000000000000, 0.000000000000000000, -1.000000000000000000 ) ) ;
#7543 = ORIENTED_EDGE ( 'NONE', *, *, #8244, .F. ) ;
#7544 = VERTEX_POINT ( 'NONE', #21335 ) ;
#7545 = EDGE_CURVE ( 'NONE', #25452, #5651, #11343, .T. ) ;
#7546 = CARTESIAN_POINT ( 'NONE',  ( 18.84633213526256768, 23.34175242840538900, 6.557713274934320324 ) ) ;
#7547 = CARTESIAN_POINT ( 'NONE',  ( 3.756430356250003211, 26.04062499938548925, 8.999999999999992895 ) ) ;
#7548 =( BOUNDED_CURVE ( )  B_SPLINE_CURVE ( 2, ( #7893, #16412, #9860, #15882, #23856, #23984, #6067, #22015, #4095 ),
 .UNSPECIFIED., .F., .F. ) 
 B_SPLINE_CURVE_WITH_KNOTS ( ( 3, 2, 2, 2, 3 ),
 ( 0.1250000000000000000, 0.1333333333333333315, 0.1499999999999999944, 0.1666666666666666574, 0.1749999999999999889 ),
 .UNSPECIFIED. ) 
 CURVE ( )  GEOMETRIC_REPRESENTATION_ITEM ( )  RATIONAL_B_SPLINE_CURVE ( ( 0.9330127018922194093, 0.9330127018922194093, 1.000000000000000000, 0.8660254037844387076, 1.000000000000000000, 0.8660254037844387076, 1.000000000000000000, 0.9330127018922194093, 0.9330127018922194093 ) ) 
 REPRESENTATION_ITEM ( '' )  );
#7549 = CIRCLE ( 'NONE', #12138, 0.4999999999999997224 ) ;
#7550 = CARTESIAN_POINT ( 'NONE',  ( 3.756430356250003211, -6.831223922626973533, 1.078124999385482230 ) ) ;
#7551 = ADVANCED_FACE ( 'NONE', ( #3415 ), #23288, .T. ) ;
#7552 = AXIS2_PLACEMENT_3D ( 'NONE', #8863, #22849, #4923 ) ;
#7553 = CIRCLE ( 'NONE', #4626, 0.4999999999999993894 ) ;
#7554 = CARTESIAN_POINT ( 'NONE',  ( 1.878215178125004048, -5.746835883940462963, 3.478124999385483029 ) ) ;
#7555 =( LENGTH_UNIT ( ) NAMED_UNIT ( * ) SI_UNIT ( .MILLI., .METRE. ) );
#7556 = VECTOR ( 'NONE', #22573, 1000.000000000000000 ) ;
#7557 = FACE_OUTER_BOUND ( 'NONE', #18946, .T. ) ;
#7558 = CIRCLE ( 'NONE', #5047, 30.10000000000000142 ) ;
#7559 = CARTESIAN_POINT ( 'NONE',  ( 1.071796769724490783, 28.50759618943234130, 12.99999999999999467 ) ) ;
#7560 = FACE_OUTER_BOUND ( 'NONE', #6321, .T. ) ;
#7561 = CARTESIAN_POINT ( 'NONE',  ( 0.000000000000000000, 0.000000000000000000, 19.50000000000000000 ) ) ;
#7562 = DIRECTION ( 'NONE',  ( 0.000000000000000000, 1.000000000000000000, 0.000000000000000000 ) ) ;
#7563 = CARTESIAN_POINT ( 'NONE',  ( 26.49999999999999645, -0.5000000000000000000, 19.50000000000000000 ) ) ;
#7564 = CARTESIAN_POINT ( 'NONE',  ( 18.19474136253732865, 18.19474136253726471, 13.61880215351699874 ) ) ;
#7565 = ORIENTED_EDGE ( 'NONE', *, *, #2001, .F. ) ;
#7566 = CARTESIAN_POINT ( 'NONE',  ( -3.999999999999996447, 27.47499999999999787, 8.999999999999992895 ) ) ;
#7567 = DIRECTION ( 'NONE',  ( 0.000000000000000000, -0.000000000000000000, -1.000000000000000000 ) ) ;
#7568 = CARTESIAN_POINT ( 'NONE',  ( 3.756430356250002323, 27.46562499938548640, 11.16877607737301226 ) ) ;
#7569 = CARTESIAN_POINT ( 'NONE',  ( -27.10000000000000497, -0.5999999999999998668, 19.59999999999999787 ) ) ;
#7570 = VECTOR ( 'NONE', #24503, 1000.000000000000000 ) ;
#7571 = CARTESIAN_POINT ( 'NONE',  ( 4.000000000000001776, -11.30940107675849760, 4.462500000000000355 ) ) ;
#7572 = CARTESIAN_POINT ( 'NONE',  ( 1.859271017917182139E-15, 28.88124999877096499, 12.99999999999999289 ) ) ;
#7573 = ORIENTED_EDGE ( 'NONE', *, *, #2294, .T. ) ;
#7574 = CARTESIAN_POINT ( 'NONE',  ( -1.878215178124998275, 29.60312499938548925, 12.25316411605951927 ) ) ;
#7575 = CARTESIAN_POINT ( 'NONE',  ( 17.87326343783943017, 25.45105997952919097, -2.750000000000000000 ) ) ;
#7577 = ORIENTED_EDGE ( 'NONE', *, *, #12078, .T. ) ;
#7576 = FACE_OUTER_BOUND ( 'NONE', #14240, .T. ) ;
#7578 = CIRCLE ( 'NONE', #20088, 4.000000000000000000 ) ;
#7579 = CIRCLE ( 'NONE', #8402, 0.5000000000000003331 ) ;
#7580 = VERTEX_POINT ( 'NONE', #3279 ) ;
#7581 = EDGE_CURVE ( 'NONE', #1055, #17423, #6752, .T. ) ;
#7582 = VERTEX_POINT ( 'NONE', #12841 ) ;
#7583 = ORIENTED_EDGE ( 'NONE', *, *, #16902, .T. ) ;
#7584 = ORIENTED_EDGE ( 'NONE', *, *, #10727, .T. ) ;
#7585 = DIRECTION ( 'NONE',  ( 1.000000000000000000, 0.000000000000000000, 0.000000000000000000 ) ) ;
#7587 = CARTESIAN_POINT ( 'NONE',  ( 0.000000000000000000, 0.000000000000000000, -6.500000000000000000 ) ) ;
#7586 = AXIS2_PLACEMENT_3D ( 'NONE', #2965, #16697, #6757 ) ;
#7588 = EDGE_CURVE ( 'NONE', #23573, #9107, #9071, .T. ) ;
#7589 = CARTESIAN_POINT ( 'NONE',  ( -23.96296185032681336, 19.82388608118453632, -6.500000000000000000 ) ) ;
#7590 = EDGE_CURVE ( 'NONE', #13124, #486, #9311, .T. ) ;
#7591 = AXIS2_PLACEMENT_3D ( 'NONE', #24891, #6969, #14949 ) ;
#7592 = CARTESIAN_POINT ( 'NONE',  ( 1.878215178125000939, -12.25316411605952283, 3.215624999385484184 ) ) ;
#7593 = CARTESIAN_POINT ( 'NONE',  ( -1.999999999999998224, -12.46410161513774639, 2.943749998770967657 ) ) ;
#7594 = CIRCLE ( 'NONE', #24736, 31.10000000000000142 ) ;
#7595 = CARTESIAN_POINT ( 'NONE',  ( 1.878215178125000939, 27.42812499938548498, 12.25316411605952283 ) ) ;
#7596 = VECTOR ( 'NONE', #21353, 1000.000000000000000 ) ;
#7597 = CARTESIAN_POINT ( 'NONE',  ( 3.469446951953614189E-15, -8.999999999999992895, 0.000000000000000000 ) ) ;
#7598 = CARTESIAN_POINT ( 'NONE',  ( 0.4995657836784154204, 38.49999999999999289, 3.020833333333325044 ) ) ;
#7599 = CARTESIAN_POINT ( 'NONE',  ( -3.999999999999996447, -8.999999999999992895, 2.474999999999997868 ) ) ;
#7600 = CARTESIAN_POINT ( 'NONE',  ( 0.000000000000000000, 0.000000000000000000, -6.500000000000000000 ) ) ;
#7601 = DIRECTION ( 'NONE',  ( 0.000000000000000000, 0.000000000000000000, -1.000000000000000000 ) ) ;
#7602 = CARTESIAN_POINT ( 'NONE',  ( 1.071796769724498111, 27.60759618943233207, 12.99999999999998757 ) ) ;
#7603 = CARTESIAN_POINT ( 'NONE',  ( -4.000000000000003553, -27.23124999877096997, 6.690598923241489970 ) ) ;
#7604 = AXIS2_PLACEMENT_3D ( 'NONE', #19723, #17384, #5222 ) ;
#7605 = CARTESIAN_POINT ( 'NONE',  ( 2.672651547586948120E-15, 28.74062499938548498, 13.33755215474602984 ) ) ;
#7606 = CARTESIAN_POINT ( 'NONE',  ( 0.000000000000000000, 10.00000000000000000, 13.00000000000000178 ) ) ;
#7607 = CARTESIAN_POINT ( 'NONE',  ( -14.54246377227319442, 27.49048467073874491, -2.750000000000000000 ) ) ;
#7608 = VERTEX_POINT ( 'NONE', #11394 ) ;
#7609 = DIRECTION ( 'NONE',  ( 0.000000000000000000, -1.000000000000000000, 0.000000000000000000 ) ) ;
#7610 = ORIENTED_EDGE ( 'NONE', *, *, #22730, .T. ) ;
#7611 = AXIS2_PLACEMENT_3D ( 'NONE', #25365, #9538, #19598 ) ;
#7612 = ORIENTED_EDGE ( 'NONE', *, *, #4182, .T. ) ;
#7613 = CARTESIAN_POINT ( 'NONE',  ( -3.834746474454188013E-15, -28.65624999877096712, 4.999999999999992006 ) ) ;
#7614 = VERTEX_POINT ( 'NONE', #21583 ) ;
#7615 = CARTESIAN_POINT ( 'NONE',  ( 3.756430356249997882, -29.11562499938548143, 11.16877607737301226 ) ) ;
#7616 = EDGE_LOOP ( 'NONE', ( #20823, #18587, #4645, #21349 ) ) ;
#7617 = CARTESIAN_POINT ( 'NONE',  ( 28.72825533807124287, -11.91206721063061913, -6.500000000000000000 ) ) ;
#7618 = AXIS2_PLACEMENT_3D ( 'NONE', #2865, #17382, #3633 ) ;
#7619 = ADVANCED_FACE ( 'NONE', ( #23940 ), #25766, .F. ) ;
#7620 = ORIENTED_EDGE ( 'NONE', *, *, #24390, .F. ) ;
#7621 = CARTESIAN_POINT ( 'NONE',  ( 2.620986760973688460E-15, 26.23750000000000071, 13.61880215351699874 ) ) ;
#7622 = CARTESIAN_POINT ( 'NONE',  ( -17.78012134629558716, 25.16042852506110705, -6.500000000000000000 ) ) ;
#7623 = EDGE_CURVE ( 'NONE', #7162, #14349, #3030, .T. ) ;
#7624 = CARTESIAN_POINT ( 'NONE',  ( 3.735045420075836212E-15, -4.662447845253954171, 1.265624999385483118 ) ) ;
#7625 = DIRECTION ( 'NONE',  ( 1.000000000000000000, 0.000000000000000000, 0.000000000000000000 ) ) ;
#7626 = CARTESIAN_POINT ( 'NONE',  ( 20.43330379829292198, 15.12090904237410527, 8.999999999999992895 ) ) ;
#7627 =( BOUNDED_CURVE ( )  B_SPLINE_CURVE ( 2, ( #6236, #16814, #4143, #235, #8206, #9898, #22693, #16179, #17884 ),
 .UNSPECIFIED., .F., .F. ) 
 B_SPLINE_CURVE_WITH_KNOTS ( ( 3, 2, 2, 2, 3 ),
 ( 0.07500000000000001110, 0.08333333333333332871, 0.1000000000000000056, 0.1166666666666666685, 0.1249999999999999861 ),
 .UNSPECIFIED. ) 
 CURVE ( )  GEOMETRIC_REPRESENTATION_ITEM ( )  RATIONAL_B_SPLINE_CURVE ( ( 0.9330127018922192983, 0.9330127018922194093, 1.000000000000000000, 0.8660254037844387076, 1.000000000000000000, 0.8660254037844387076, 1.000000000000000000, 0.9330127018922195203, 0.9330127018922194093 ) ) 
 REPRESENTATION_ITEM ( '' )  );
#7628 = CARTESIAN_POINT ( 'NONE',  ( -5.827558883615604479, 30.54913349766230724, 1.000000000000000000 ) ) ;
#7629 =( GEOMETRIC_REPRESENTATION_CONTEXT ( 3 ) GLOBAL_UNCERTAINTY_ASSIGNED_CONTEXT ( ( #24841 ) ) GLOBAL_UNIT_ASSIGNED_CONTEXT ( ( #15539, #8073, #17622 ) ) REPRESENTATION_CONTEXT ( 'NONE', 'WORKASPACE' ) );
#7630 = CARTESIAN_POINT ( 'NONE',  ( -1.999999999999995781, 27.40000000000000213, 5.535898384862237620 ) ) ;
#7631 = EDGE_CURVE ( 'NONE', #4731, #19766, #6778, .T. ) ;
#7632 = CIRCLE ( 'NONE', #20588, 0.5000000000000000000 ) ;
#7633 = CARTESIAN_POINT ( 'NONE',  ( 4.000000000000001776, 25.86250000000000071, 11.30940107675849760 ) ) ;
#7634 = CARTESIAN_POINT ( 'NONE',  ( 2.000000000000000000, 28.07500000000000995, 12.46410161513774817 ) ) ;
#7635 = ORIENTED_EDGE ( 'NONE', *, *, #10998, .F. ) ;
#7636 = ORIENTED_EDGE ( 'NONE', *, *, #16361, .F. ) ;
#7637 = CARTESIAN_POINT ( 'NONE',  ( 1.878215178125003382, 25.32812499938548356, 5.746835883940462963 ) ) ;
#7638 = ORIENTED_EDGE ( 'NONE', *, *, #11592, .T. ) ;
#7639 = CARTESIAN_POINT ( 'NONE',  ( -25.45105997952899912, 17.87326343783971083, -2.750000000000000000 ) ) ;
#7640 = CARTESIAN_POINT ( 'NONE',  ( 3.735045420075836212E-15, 27.61562499938548498, 4.662447845253954171 ) ) ;
#7641 = DIRECTION ( 'NONE',  ( 0.9822872507286911636, 0.1873813145857119722, 0.000000000000000000 ) ) ;
#7642 = ORIENTED_EDGE ( 'NONE', *, *, #21118, .T. ) ;
#7643 = ORIENTED_EDGE ( 'NONE', *, *, #15801, .T. ) ;
#7644 = VECTOR ( 'NONE', #6709, 1000.000000000000000 ) ;
#7645 = DIRECTION ( 'NONE',  ( 1.000000000000000000, 0.000000000000000000, 0.000000000000000000 ) ) ;
#7646 = ORIENTED_EDGE ( 'NONE', *, *, #4698, .F. ) ;
#7647 = CARTESIAN_POINT ( 'NONE',  ( -1.998723687422152831E-12, 39.00000000001113420, 14.49999999998978240 ) ) ;
#7648 = EDGE_CURVE ( 'NONE', #13124, #20633, #12431, .T. ) ;
#7649 = DIRECTION ( 'NONE',  ( 1.000000000000000000, 0.000000000000000000, 0.000000000000000000 ) ) ;
#7650 = CARTESIAN_POINT ( 'NONE',  ( -1.878215178124998275, 28.14062499938548711, 12.25316411605951927 ) ) ;
#7651 = CARTESIAN_POINT ( 'NONE',  ( -1.859271017917182139E-15, -26.68750000000000000, 12.99999999999999289 ) ) ;
#7652 = CARTESIAN_POINT ( 'NONE',  ( 4.000000000000002665, 27.66249999999999787, 11.30940107675849760 ) ) ;
#7653 = EDGE_CURVE ( 'NONE', #14487, #9154, #3544, .T. ) ;
#7654 = COLOUR_RGB ( '',0.8941176470588234615, 0.8941176470588234615, 0.8941176470588234615 ) ;
#7655 = CARTESIAN_POINT ( 'NONE',  ( -1.878215178124995832, 27.99062499938548143, 5.746835883940462963 ) ) ;
#7656 = LINE ( 'NONE', #13666, #1675 ) ;
#7657 = EDGE_CURVE ( 'NONE', #11405, #11752, #13472, .T. ) ;
#7658 = CARTESIAN_POINT ( 'NONE',  ( 0.000000000000000000, 0.000000000000000000, -6.500000000000000000 ) ) ;
#7659 = VECTOR ( 'NONE', #3119, 1000.000000000000000 ) ;
#7660 = CARTESIAN_POINT ( 'NONE',  ( 2.672651547586948120E-15, 28.62812499938548783, 13.33755215474603162 ) ) ;
#7661 = PLANE ( 'NONE',  #7055 ) ;
#7662 = CARTESIAN_POINT ( 'NONE',  ( 21.77888886054569539, 16.12203461105324820, 8.999999999999992895 ) ) ;
#7663 = CARTESIAN_POINT ( 'NONE',  ( 22.42204162038009230, 17.10964686446126848, 8.999999999999992895 ) ) ;
#7664 = DIRECTION ( 'NONE',  ( 0.000000000000000000, 0.000000000000000000, -1.000000000000000000 ) ) ;
#7665 = CARTESIAN_POINT ( 'NONE',  ( 1.071796769724492338, 29.35134618820330488, 12.99999999999999467 ) ) ;
#7666 = DIRECTION ( 'NONE',  ( -0.000000000000000000, -0.000000000000000000, -1.000000000000000000 ) ) ;
#7667 = CARTESIAN_POINT ( 'NONE',  ( 18.14379053194667790, 23.45618528786534895, 8.999999999999992895 ) ) ;
#7668 = DIRECTION ( 'NONE',  ( 1.000000000000000000, 0.000000000000000000, 0.000000000000000000 ) ) ;
#7669 = ORIENTED_EDGE ( 'NONE', *, *, #18367, .T. ) ;
#7670 = CARTESIAN_POINT ( 'NONE',  ( 2.000000000000000888, 26.21874999877096712, 12.46410161513774817 ) ) ;
#7671 = CARTESIAN_POINT ( 'NONE',  ( -2.000000000000000888, -26.27499999999999858, 12.46410161513774817 ) ) ;
#7673 = VERTEX_POINT ( 'NONE', #11517 ) ;
#7672 = CARTESIAN_POINT ( 'NONE',  ( -3.756430356249997882, 25.51562499938549067, 11.16877607737301048 ) ) ;
#7674 = CARTESIAN_POINT ( 'NONE',  ( 1.878215178125004048, 28.02812499938548640, 5.746835883940462963 ) ) ;
#7675 = CARTESIAN_POINT ( 'NONE',  ( -27.49048467073863833, -14.54246377227340048, 1.000000000000000000 ) ) ;
#7676 =( GEOMETRIC_REPRESENTATION_CONTEXT ( 3 ) GLOBAL_UNCERTAINTY_ASSIGNED_CONTEXT ( ( #10971 ) ) GLOBAL_UNIT_ASSIGNED_CONTEXT ( ( #231, #7808, #11863 ) ) REPRESENTATION_CONTEXT ( 'NONE', 'WORKASPACE' ) );
#7677 = ORIENTED_EDGE ( 'NONE', *, *, #23921, .T. ) ;
#7678 = FACE_OUTER_BOUND ( 'NONE', #6418, .T. ) ;
#7679 = ORIENTED_EDGE ( 'NONE', *, *, #44, .T. ) ;
#7680 = ORIENTED_EDGE ( 'NONE', *, *, #22902, .F. ) ;
#7681 = CARTESIAN_POINT ( 'NONE',  ( -3.756430356249997882, 26.26562499938548711, 8.999999999999992895 ) ) ;
#7682 = CIRCLE ( 'NONE', #22607, 4.000000000000000000 ) ;
#7683 = CARTESIAN_POINT ( 'NONE',  ( 2.672651547586948120E-15, -13.33755215474603162, 4.078124999385480010 ) ) ;
#7684 = EDGE_CURVE ( 'NONE', #9053, #7861, #11361, .T. ) ;
#7685 = CARTESIAN_POINT ( 'NONE',  ( -1.071796769724485454, 27.51115380933863719, 12.99999999999999467 ) ) ;
#7686 = CARTESIAN_POINT ( 'NONE',  ( 0.4995657836784084815, 34.50000000000000000, 14.97916666666665897 ) ) ;
#7687 = ADVANCED_FACE ( 'NONE', ( #3663 ), #15587, .F. ) ;
#7688 = CARTESIAN_POINT ( 'NONE',  ( 2.000000000000000000, 28.52500000000000924, 12.46410161513774817 ) ) ;
#7689 = CARTESIAN_POINT ( 'NONE',  ( 0.5000000000000001110, 6.123233995736767268E-17, 16.00000000000000000 ) ) ;
#7690 = PRODUCT_DEFINITION_FORMATION_WITH_SPECIFIED_SOURCE ( 'ANY', '', #2546, .NOT_KNOWN. ) ;
#7691 = EDGE_CURVE ( 'NONE', #9386, #20150, #17221, .T. ) ;
#7692 = CARTESIAN_POINT ( 'NONE',  ( -19.82388608118446527, -23.96296185032687376, -6.500000000000000000 ) ) ;
#7693 = DIRECTION ( 'NONE',  ( 1.000000000000000000, 0.000000000000000000, 0.000000000000000000 ) ) ;
#7694 = DIRECTION ( 'NONE',  ( 0.000000000000000000, 0.000000000000000000, 1.000000000000000000 ) ) ;
#7695 = CARTESIAN_POINT ( 'NONE',  ( 17.60253943329360382, 20.43096655803972084, 5.535898384862237620 ) ) ;
#7696 = VERTEX_POINT ( 'NONE', #11641 ) ;
#7697 = DIRECTION ( 'NONE',  ( 0.000000000000000000, 0.000000000000000000, 1.000000000000000000 ) ) ;
#7698 = CARTESIAN_POINT ( 'NONE',  ( 1.878215178124995832, -28.55312499938548498, 5.746835883940462963 ) ) ;
#7699 = CARTESIAN_POINT ( 'NONE',  ( 3.756430356250004099, 27.99062499938548498, 6.831223922626973533 ) ) ;
#7700 = FACE_OUTER_BOUND ( 'NONE', #19653, .T. ) ;
#7701 = DIRECTION ( 'NONE',  ( -0.000000000000000000, -1.000000000000000000, -0.000000000000000000 ) ) ;
#7702 = CARTESIAN_POINT ( 'NONE',  ( 1.071796769724487675, 29.08615380933863293, 4.999999999999988454 ) ) ;
#7703 = VERTEX_POINT ( 'NONE', #21716 ) ;
#7704 = CARTESIAN_POINT ( 'NONE',  ( 1.071796769724495668, 27.15759618943233633, 12.99999999999999112 ) ) ;
#7705 = ADVANCED_FACE ( 'NONE', ( #19870 ), #5638, .T. ) ;
#7706 = LINE ( 'NONE', #9912, #24219 ) ;
#7708 = ORIENTED_EDGE ( 'NONE', *, *, #13171, .F. ) ;
#7707 = DIRECTION ( 'NONE',  ( 0.9510565162951586382, 0.3090169943749320192, 0.000000000000000000 ) ) ;
#7709 = VERTEX_POINT ( 'NONE', #13877 ) ;
#7710 = ORIENTED_EDGE ( 'NONE', *, *, #11535, .F. ) ;
#7711 = ORIENTED_EDGE ( 'NONE', *, *, #21354, .T. ) ;
#7712 = EDGE_LOOP ( 'NONE', ( #8550, #12792, #10850, #6843 ) ) ;
#7713 = CARTESIAN_POINT ( 'NONE',  ( -29.41953157733101065, -10.08469938919468945, -2.750000000000000000 ) ) ;
#7714 = FACE_OUTER_BOUND ( 'NONE', #24075, .T. ) ;
#7715 = CARTESIAN_POINT ( 'NONE',  ( 1.071796769724493448, -29.18259618943233136, 4.999999999999995559 ) ) ;
#7716 = ADVANCED_FACE ( 'NONE', ( #19616 ), #23422, .T. ) ;
#7717 = CARTESIAN_POINT ( 'NONE',  ( -3.756430356249996105, 25.40312499938548640, 11.16877607737301226 ) ) ;
#7718 = CARTESIAN_POINT ( 'NONE',  ( -3.756430356249997882, -11.16877607737301226, 4.003124999385478056 ) ) ;
#7719 = CARTESIAN_POINT ( 'NONE',  ( 3.752267015613588906E-15, -4.381197846482986158, 4.556249998770967480 ) ) ;
#7720 = CARTESIAN_POINT ( 'NONE',  ( 0.000000000000000000, 0.000000000000000000, 0.000000000000000000 ) ) ;
#7721 = CARTESIAN_POINT ( 'NONE',  ( -3.756430356249997882, 27.76562499938549067, 11.16877607737301226 ) ) ;
#7722 = DIRECTION ( 'NONE',  ( 1.000000000000000000, 0.000000000000000000, 0.000000000000000000 ) ) ;
#7723 = CARTESIAN_POINT ( 'NONE',  ( 20.28643891059321902, 21.80218843844518872, 12.99999999999999289 ) ) ;
#7724 = CARTESIAN_POINT ( 'NONE',  ( 4.000000000000003553, -6.690598923241489970, 2.287499999999995648 ) ) ;
#7725 = FACE_OUTER_BOUND ( 'NONE', #17657, .T. ) ;
#7726 = CARTESIAN_POINT ( 'NONE',  ( 2.000000000000005329, 27.77500000000000568, 5.535898384862238508 ) ) ;
#7727 = EDGE_CURVE ( 'NONE', #4195, #8387, #1720, .T. ) ;
#7728 = CARTESIAN_POINT ( 'NONE',  ( -2.000000000000000888, -27.11874999877096926, 12.46410161513774817 ) ) ;
#7729 = CARTESIAN_POINT ( 'NONE',  ( 3.756430356250002323, 28.81562499938548427, 11.16877607737301226 ) ) ;
#7730 = LINE ( 'NONE', #19761, #22474 ) ;
#7731 = CARTESIAN_POINT ( 'NONE',  ( 3.752267015613588906E-15, -4.381197846482986158, 3.206249998770963838 ) ) ;
#7732 = CARTESIAN_POINT ( 'NONE',  ( 0.000000000000000000, 0.000000000000000000, -6.500000000000000000 ) ) ;
#7733 = VERTEX_POINT ( 'NONE', #5509 ) ;
#7734 = EDGE_CURVE ( 'NONE', #10526, #16921, #9283, .T. ) ;
#7735 = CARTESIAN_POINT ( 'NONE',  ( 2.000000000000003997, 25.46874999877096712, 5.535898384862238508 ) ) ;
#7736 = VERTEX_POINT ( 'NONE', #19757 ) ;
#7737 = EDGE_CURVE ( 'NONE', #14144, #13306, #1854, .T. ) ;
#7738 = VERTEX_POINT ( 'NONE', #14514 ) ;
#7739 = DIRECTION ( 'NONE',  ( 1.000000000000000000, 0.000000000000000000, 0.000000000000000000 ) ) ;
#7740 = EDGE_LOOP ( 'NONE', ( #8481, #20152, #15430 ) ) ;
#7741 = CARTESIAN_POINT ( 'NONE',  ( 3.756430356249996994, -28.17812499938548498, 8.999999999999992895 ) ) ;
#7742 = ORIENTED_EDGE ( 'NONE', *, *, #9266, .T. ) ;
#7743 = CARTESIAN_POINT ( 'NONE',  ( -1.071796769724493448, 28.73259618943232852, 4.999999999999995559 ) ) ;
#7744 = VERTEX_POINT ( 'NONE', #2357 ) ;
#7745 = CARTESIAN_POINT ( 'NONE',  ( 4.000000000000003553, 27.70000000000000284, 8.999999999999992895 ) ) ;
#7746 = CARTESIAN_POINT ( 'NONE',  ( 2.000000000000000000, 29.42500000000000426, 12.46410161513774817 ) ) ;
#7747 = VECTOR ( 'NONE', #3246, 1000.000000000000000 ) ;
#7748 = CYLINDRICAL_SURFACE ( 'NONE', #13845, 0.5000000000000004441 ) ;
#7749 = DIRECTION ( 'NONE',  ( -0.000000000000000000, -1.000000000000000000, -0.000000000000000000 ) ) ;
#7750 = VECTOR ( 'NONE', #558, 1000.000000000000000 ) ;
#7751 = CARTESIAN_POINT ( 'NONE',  ( 17.93165849759071762, 23.24405325350938867, 11.16877607737301226 ) ) ;
#7752 = DIRECTION ( 'NONE',  ( -1.000000000000000000, 0.000000000000000000, 0.000000000000000000 ) ) ;
#7753 = CARTESIAN_POINT ( 'NONE',  ( 11.44867358849351113, 28.91604871112461339, -6.500000000000000000 ) ) ;
#7754 = CARTESIAN_POINT ( 'NONE',  ( -1.999999999999998224, 27.55000000000000071, 12.46410161513774639 ) ) ;
#7755 = CARTESIAN_POINT ( 'NONE',  ( 4.000000000000003553, -8.999999999999992895, 18.00000000000000000 ) ) ;
#7756 = CARTESIAN_POINT ( 'NONE',  ( 22.31370212894720240, 19.65750475098775496, 12.25316411605952283 ) ) ;
#7757 = DIRECTION ( 'NONE',  ( -0.6845471059286831750, 0.7289686274214168815, 0.000000000000000000 ) ) ;
#7758 = ORIENTED_EDGE ( 'NONE', *, *, #7302, .T. ) ;
#7759 = EDGE_CURVE ( 'NONE', #19902, #8252, #20129, .T. ) ;
#7760 = VERTEX_POINT ( 'NONE', #18190 ) ;
#7761 = CARTESIAN_POINT ( 'NONE',  ( -1.878215178124998275, 26.00312499938549493, 12.25316411605951927 ) ) ;
#7762 = EDGE_CURVE ( 'NONE', #18701, #11472, #16218, .T. ) ;
#7763 = EDGE_LOOP ( 'NONE', ( #1803, #3619, #18452, #17108 ) ) ;
#7764 = CARTESIAN_POINT ( 'NONE',  ( 4.000000000000003553, 26.35000000000000142, 8.999999999999992895 ) ) ;
#7765 = CARTESIAN_POINT ( 'NONE',  ( 17.07220934740368889, 19.90063647214981302, 12.46410161513774639 ) ) ;
#7766 = CARTESIAN_POINT ( 'NONE',  ( 15.00834143068450999, 20.66519568017682573, 8.999999999999992895 ) ) ;
#7767 = ORIENTED_EDGE ( 'NONE', *, *, #18911, .F. ) ;
#7768 = VERTEX_POINT ( 'NONE', #2478 ) ;
#7769 =( BOUNDED_CURVE ( )  B_SPLINE_CURVE ( 2, ( #6468, #10366, #2544, #467, #12617, #20717, #18511, #16548, #10762, #24507, #6721, #6589, #14573, #22555, #716, #18750, #842, #5026, #2934, #17439, #3310, #19265, #23078, #19133, #13141, #1097, #3184, #25289, #23194, #11286, #23453, #3449, #5162, #20989, #979, #1224, #7118, #1488, #11152, #7492, #6981, #13006, #8960, #25168, #9461, #5279, #10896, #9341, #3066, #7249, #15229, #1368, #13255, #15486, #21227, #16935, #15102, #17325, #25406, #9206, #12867, #21106, #20844, #11423, #18896, #17196, #7369, #15346, #13394, #23316, #19397, #21370, #5406, #24904, #14962, #11034, #22939, #19013, #9073, #17056, #25025, #3833, #15617, #21881, #4081, #9845, #17827, #12054, #9585, #3574, #15867, #11675, #23702, #5543, #9970, #13526, #23584, #1612, #16131, #1883, #20036, #2139, #18104, #25798, #9727, #13912, #10102, #11813, #5666, #3694, #11545, #14037, #21752, #17961, #1757, #19651, #19899, #6054, #7756, #16007, #17708 ),
 .UNSPECIFIED., .F., .F. ) 
 B_SPLINE_CURVE_WITH_KNOTS ( ( 3, 2, 2, 2, 2, 2, 2, 2, 2, 2, 2, 2, 2, 2, 2, 2, 2, 2, 2, 2, 2, 2, 2, 2, 2, 2, 2, 2, 2, 2, 2, 2, 2, 2, 2, 2, 2, 2, 2, 2, 2, 2, 2, 2, 2, 2, 2, 2, 2, 2, 2, 2, 2, 2, 2, 2, 2, 2, 2, 2, 3 ),
 ( 0.000000000000000000, 0.01666666666666666644, 0.03333333333333333287, 0.05000000000000000278, 0.06666666666666666574, 0.08333333333333332871, 0.1000000000000000056, 0.1166666666666666685, 0.1333333333333333315, 0.1499999999999999944, 0.1666666666666666574, 0.1833333333333333204, 0.2000000000000000111, 0.2166666666666666741, 0.2333333333333333370, 0.2500000000000000000, 0.2666666666666666630, 0.2833333333333333259, 0.2999999999999999889, 0.3166666666666666519, 0.3333333333333333148, 0.3499999999999999778, 0.3666666666666666408, 0.3833333333333333592, 0.4000000000000000222, 0.4166666666666666852, 0.4333333333333333481, 0.4500000000000000111, 0.4666666666666666741, 0.4833333333333333370, 0.5000000000000000000, 0.5166666666666667185, 0.5333333333333333259, 0.5500000000000000444, 0.5666666666666666519, 0.5833333333333333703, 0.5999999999999999778, 0.6166666666666666963, 0.6333333333333333037, 0.6500000000000000222, 0.6666666666666666297, 0.6833333333333333481, 0.6999999999999999556, 0.7166666666666666741, 0.7333333333333332815, 0.7500000000000000000, 0.7666666666666667185, 0.7833333333333333259, 0.8000000000000000444, 0.8166666666666666519, 0.8333333333333333703, 0.8499999999999999778, 0.8666666666666666963, 0.8833333333333333037, 0.9000000000000000222, 0.9166666666666666297, 0.9333333333333333481, 0.9499999999999999556, 0.9666666666666666741, 0.9833333333333332815, 1.000000000000000000 ),
 .UNSPECIFIED. ) 
 CURVE ( )  GEOMETRIC_REPRESENTATION_ITEM ( )  RATIONAL_B_SPLINE_CURVE ( ( 1.000000000000000000, 0.8660254037844387076, 1.000000000000000000, 0.8660254037844387076, 1.000000000000000000, 0.8660254037844387076, 1.000000000000000000, 0.8660254037844387076, 1.000000000000000000, 0.8660254037844387076, 1.000000000000000000, 0.8660254037844387076, 1.000000000000000000, 0.8660254037844387076, 1.000000000000000000, 0.8660254037844387076, 1.000000000000000000, 0.8660254037844387076, 1.000000000000000000, 0.8660254037844387076, 1.000000000000000000, 0.8660254037844387076, 1.000000000000000000, 0.8660254037844387076, 1.000000000000000000, 0.8660254037844387076, 1.000000000000000000, 0.8660254037844387076, 1.000000000000000000, 0.8660254037844387076, 1.000000000000000000, 0.8660254037844387076, 1.000000000000000000, 0.8660254037844387076, 1.000000000000000000, 0.8660254037844387076, 1.000000000000000000, 0.8660254037844387076, 1.000000000000000000, 0.8660254037844387076, 1.000000000000000000, 0.8660254037844387076, 1.000000000000000000, 0.8660254037844387076, 1.000000000000000000, 0.8660254037844387076, 1.000000000000000000, 0.8660254037844387076, 1.000000000000000000, 0.8660254037844387076, 1.000000000000000000, 0.8660254037844387076, 1.000000000000000000, 0.8660254037844387076, 1.000000000000000000, 0.8660254037844387076, 1.000000000000000000, 0.8660254037844387076, 1.000000000000000000, 0.8660254037844387076, 1.000000000000000000, 0.8660254037844387076, 1.000000000000000000, 0.8660254037844387076, 1.000000000000000000, 0.8660254037844387076, 1.000000000000000000, 0.8660254037844387076, 1.000000000000000000, 0.8660254037844387076, 1.000000000000000000, 0.8660254037844387076, 1.000000000000000000, 0.8660254037844387076, 1.000000000000000000, 0.8660254037844387076, 1.000000000000000000, 0.8660254037844387076, 1.000000000000000000, 0.8660254037844387076, 1.000000000000000000, 0.8660254037844387076, 1.000000000000000000, 0.8660254037844387076, 1.000000000000000000, 0.8660254037844387076, 1.000000000000000000, 0.8660254037844387076, 1.000000000000000000, 0.8660254037844387076, 1.000000000000000000, 0.8660254037844387076, 1.000000000000000000, 0.8660254037844387076, 1.000000000000000000, 0.8660254037844387076, 1.000000000000000000, 0.8660254037844387076, 1.000000000000000000, 0.8660254037844387076, 1.000000000000000000, 0.8660254037844387076, 1.000000000000000000, 0.8660254037844387076, 1.000000000000000000, 0.8660254037844387076, 1.000000000000000000, 0.8660254037844387076, 1.000000000000000000, 0.8660254037844387076, 1.000000000000000000, 0.8660254037844387076, 1.000000000000000000, 0.8660254037844387076, 1.000000000000000000, 0.8660254037844387076, 1.000000000000000000, 0.8660254037844387076, 1.000000000000000000, 0.8660254037844387076, 1.000000000000000000 ) ) 
 REPRESENTATION_ITEM ( '' )  );
#7770 = EDGE_CURVE ( 'NONE', #4455, #10488, #8028, .T. ) ;
#7771 = DIRECTION ( 'NONE',  ( -0.000000000000000000, 0.000000000000000000, 1.000000000000000000 ) ) ;
#7772 = VERTEX_POINT ( 'NONE', #22356 ) ;
#7773 = CARTESIAN_POINT ( 'NONE',  ( 3.202063662808456446, 39.00157412423376968, 4.529845232042116976 ) ) ;
#7774 = PLANE ( 'NONE',  #10516 ) ;
#7775 =( BOUNDED_CURVE ( )  B_SPLINE_CURVE ( 2, ( #10113, #18114, #17714, #189, #21620, #3703, #11684, #23709, #5795 ),
 .UNSPECIFIED., .F., .F. ) 
 B_SPLINE_CURVE_WITH_KNOTS ( ( 3, 2, 2, 2, 3 ),
 ( 0.9250000000000000444, 0.9333333333333333481, 0.9499999999999999556, 0.9666666666666666741, 0.9749999999999999778 ),
 .UNSPECIFIED. ) 
 CURVE ( )  GEOMETRIC_REPRESENTATION_ITEM ( )  RATIONAL_B_SPLINE_CURVE ( ( 0.9330127018922194093, 0.9330127018922198534, 1.000000000000000000, 0.8660254037844387076, 1.000000000000000000, 0.8660254037844387076, 1.000000000000000000, 0.9330127018922194093, 0.9330127018922194093 ) ) 
 REPRESENTATION_ITEM ( '' )  );
#7776 = CARTESIAN_POINT ( 'NONE',  ( -3.756430356250000546, 28.55312499938548854, 11.16877607737301048 ) ) ;
#7777 = DIRECTION ( 'NONE',  ( -0.000000000000000000, -1.000000000000000000, -0.000000000000000000 ) ) ;
#7778 = CARTESIAN_POINT ( 'NONE',  ( -1.999999999999998224, 26.95000000000000639, 5.535898384862237620 ) ) ;
#7779 = CARTESIAN_POINT ( 'NONE',  ( 3.756430356250002323, 25.55312499938548143, 11.16877607737301226 ) ) ;
#7780 = SURFACE_SIDE_STYLE ('',( #18480 ) ) ;
#7781 = CARTESIAN_POINT ( 'NONE',  ( -26.50000000000000355, -0.5000000000000000000, 19.50000000000000000 ) ) ;
#7782 = CARTESIAN_POINT ( 'NONE',  ( -3.878215178125003604, -25.32343749907822783, 8.999999999999992895 ) ) ;
#7783 = CARTESIAN_POINT ( 'NONE',  ( 22.41528496361359046, 16.75843071412113972, 8.999999999999992895 ) ) ;
#7784 = CARTESIAN_POINT ( 'NONE',  ( 18.19682354053567153, 23.50921829645433903, 6.831223922626973533 ) ) ;
#7785 = LINE ( 'NONE', #1787, #13452 ) ;
#7786 = CARTESIAN_POINT ( 'NONE',  ( 0.000000000000000000, 0.000000000000000000, 0.000000000000000000 ) ) ;
#7788 = ADVANCED_FACE ( 'NONE', ( #14398 ), #20660, .F. ) ;
#7787 = CARTESIAN_POINT ( 'NONE',  ( 1.071796769724492115, 27.28615380933864287, 4.999999999999989342 ) ) ;
#7789 = CARTESIAN_POINT ( 'NONE',  ( 26.49999999999999645, -0.5000000000000000000, 19.50000000000000000 ) ) ;
#7790 = CARTESIAN_POINT ( 'NONE',  ( 18.77930694887276886, 17.26355742102066415, 4.999999999999992006 ) ) ;
#7791 = VERTEX_POINT ( 'NONE', #20526 ) ;
#7792 = CARTESIAN_POINT ( 'NONE',  ( 2.000000000000000888, 28.46874999877097068, 12.46410161513774817 ) ) ;
#7793 = CARTESIAN_POINT ( 'NONE',  ( -4.000000000000003553, -27.28749999999999787, 6.690598923241489970 ) ) ;
#7795 = VERTEX_POINT ( 'NONE', #8242 ) ;
#7794 = CARTESIAN_POINT ( 'NONE',  ( -4.000000000000003553, -29.89374999877096784, 8.999999999999992895 ) ) ;
#7796 = CARTESIAN_POINT ( 'NONE',  ( 3.735045420075836212E-15, 29.41562499938548569, 4.662447845253954171 ) ) ;
#7797 = CYLINDRICAL_SURFACE ( 'NONE', #21372, 0.5000000000000004441 ) ;
#7798 = VERTEX_POINT ( 'NONE', #24570 ) ;
#7799 = CARTESIAN_POINT ( 'NONE',  ( 3.756430356249996994, -29.41562499938548569, 8.999999999999992895 ) ) ;
#7800 = ORIENTED_EDGE ( 'NONE', *, *, #7863, .F. ) ;
#7801 = ORIENTED_EDGE ( 'NONE', *, *, #24725, .T. ) ;
#7802 = FILL_AREA_STYLE ('',( #1805 ) ) ;
#7803 = CARTESIAN_POINT ( 'NONE',  ( -3.756430356249996105, 25.32812499938549067, 6.831223922626973533 ) ) ;
#7804 = EDGE_CURVE ( 'NONE', #10048, #702, #17788, .T. ) ;
#7805 = CARTESIAN_POINT ( 'NONE',  ( -3.756430356249996994, -8.999999999999992895, 2.165624999385482141 ) ) ;
#7806 = B_SPLINE_CURVE_WITH_KNOTS ( 'NONE', 3,
 ( #10630, #18621, #22406, #24106, #2282, #8675, #14180, #22150 ),
 .UNSPECIFIED., .F., .F.,
 ( 4, 2, 2, 4 ),
 ( 0.0009289288217882851880, 0.001160777380751508870, 0.001392625939714732444, 0.001856323057641176772 ),
 .UNSPECIFIED. ) ;
#7807 = CARTESIAN_POINT ( 'NONE',  ( -26.25859848311247902, 16.66421332384710752, -6.500000000000000000 ) ) ;
#7808 =( NAMED_UNIT ( * ) PLANE_ANGLE_UNIT ( ) SI_UNIT ( $, .RADIAN. ) );
#7809 = CARTESIAN_POINT ( 'NONE',  ( -3.999999999999996447, -8.999999999999992895, 3.824999999999998401 ) ) ;
#7810 = CARTESIAN_POINT ( 'NONE',  ( 0.000000000000000000, 0.000000000000000000, 1.000000000000000000 ) ) ;
#7811 = CARTESIAN_POINT ( 'NONE',  ( 4.648177544792955347E-16, 29.33124999877097139, 12.99999999999999289 ) ) ;
#7812 = DIRECTION ( 'NONE',  ( 0.000000000000000000, -0.000000000000000000, 1.000000000000000000 ) ) ;
#7813 = CYLINDRICAL_SURFACE ( 'NONE', #20830, 0.5000000000000004441 ) ;
#7814 = DIRECTION ( 'NONE',  ( 0.000000000000000000, -0.000000000000000000, 1.000000000000000000 ) ) ;
#7815 = CARTESIAN_POINT ( 'NONE',  ( 20.78451994863305430, 15.12766569914060888, 8.999999999999992895 ) ) ;
#7816 = ORIENTED_EDGE ( 'NONE', *, *, #714, .F. ) ;
#7817 = CARTESIAN_POINT ( 'NONE',  ( -5.206645097256043186, 38.99989214654020486, 10.77428791256852669 ) ) ;
#7818 = CARTESIAN_POINT ( 'NONE',  ( 0.2644264925860129734, 30.00000000000001421, 4.999999999999992006 ) ) ;
#7819 = CARTESIAN_POINT ( 'NONE',  ( 1.878215178125000939, 27.42812499938548498, 12.25316411605952283 ) ) ;
#7820 = FACE_OUTER_BOUND ( 'NONE', #9001, .T. ) ;
#7821 = DIRECTION ( 'NONE',  ( 0.000000000000000000, 0.000000000000000000, 1.000000000000000000 ) ) ;
#7822 = LINE ( 'NONE', #9909, #6817 ) ;
#7823 = ORIENTED_EDGE ( 'NONE', *, *, #21096, .T. ) ;
#7824 = CARTESIAN_POINT ( 'NONE',  ( 2.000000000000003997, 27.32500000000000284, 5.535898384862238508 ) ) ;
#7826 = ORIENTED_EDGE ( 'NONE', *, *, #8861, .T. ) ;
#7825 = DIRECTION ( 'NONE',  ( 0.000000000000000000, 0.000000000000000000, 1.000000000000000000 ) ) ;
#7827 = VERTEX_POINT ( 'NONE', #22485 ) ;
#7828 = VERTEX_POINT ( 'NONE', #18443 ) ;
#7830 = EDGE_CURVE ( 'NONE', #8636, #17199, #16114, .T. ) ;
#7829 = ORIENTED_EDGE ( 'NONE', *, *, #22775, .T. ) ;
#7831 = ORIENTED_EDGE ( 'NONE', *, *, #3456, .F. ) ;
#7832 = LINE ( 'NONE', #23925, #11378 ) ;
#7833 = CARTESIAN_POINT ( 'NONE',  ( -9.296355089585910693E-16, 26.91250000000000497, 4.999999999999991118 ) ) ;
#7834 = CIRCLE ( 'NONE', #22445, 30.00000000000000355 ) ;
#7835 = CYLINDRICAL_SURFACE ( 'NONE', #1833, 0.5000000000000004441 ) ;
#7836 = CARTESIAN_POINT ( 'NONE',  ( -1.878215178124996498, 27.54062499938548569, 5.746835883940462963 ) ) ;
#7837 = CARTESIAN_POINT ( 'NONE',  ( 3.756430356250004099, -6.831223922626973533, 1.978124999385481697 ) ) ;
#7838 = CARTESIAN_POINT ( 'NONE',  ( 2.000000000000003997, -5.535898384862238508, 3.618749998770966148 ) ) ;
#7839 =( NAMED_UNIT ( * ) SI_UNIT ( $, .STERADIAN. ) SOLID_ANGLE_UNIT ( ) );
#7840 = CARTESIAN_POINT ( 'NONE',  ( 3.756430356250004099, 29.34062499938548640, 6.831223922626973533 ) ) ;
#7841 = DIRECTION ( 'NONE',  ( 1.000000000000000000, 0.000000000000000000, 0.000000000000000000 ) ) ;
#7842 = DIRECTION ( 'NONE',  ( 0.000000000000000000, 0.000000000000000000, -1.000000000000000000 ) ) ;
#7843 = CARTESIAN_POINT ( 'NONE',  ( -1.999999999999995781, -5.535898384862237620, 2.849999999999998312 ) ) ;
#7844 = CARTESIAN_POINT ( 'NONE',  ( -3.469446951953614189E-15, -25.00000000000000000, 8.999999999999992895 ) ) ;
#7845 = CARTESIAN_POINT ( 'NONE',  ( 5.112995299272250684E-15, 26.40624999877096712, 4.999999999999992006 ) ) ;
#7846 = CARTESIAN_POINT ( 'NONE',  ( -7.734255490827218971, -30.12293631110037140, 1.000000000000000000 ) ) ;
#7847 = CARTESIAN_POINT ( 'NONE',  ( -4.000000000000003553, -27.64374999877096784, 8.999999999999992895 ) ) ;
#7848 = CARTESIAN_POINT ( 'NONE',  ( 1.878215178125000939, 26.97812499938548569, 12.25316411605952283 ) ) ;
#7849 = DIRECTION ( 'NONE',  ( 1.000000000000000000, 0.000000000000000000, 0.000000000000000000 ) ) ;
#7850 = CIRCLE ( 'NONE', #5354, 31.10000000000000142 ) ;
#7851 = CYLINDRICAL_SURFACE ( 'NONE', #4137, 0.5000000000000004441 ) ;
#7852 = DIRECTION ( 'NONE',  ( 1.000000000000000000, 0.000000000000000000, 0.000000000000000000 ) ) ;
#7853 = ORIENTED_EDGE ( 'NONE', *, *, #16431, .F. ) ;
#7854 = CARTESIAN_POINT ( 'NONE',  ( 3.369928719974892281E-15, 25.50624999877096855, 4.999999999999992006 ) ) ;
#7855 = ORIENTED_EDGE ( 'NONE', *, *, #21496, .T. ) ;
#7856 = ORIENTED_EDGE ( 'NONE', *, *, #4104, .F. ) ;
#7857 = DIRECTION ( 'NONE',  ( 0.000000000000000000, -0.000000000000000000, 1.000000000000000000 ) ) ;
#7859 = ORIENTED_EDGE ( 'NONE', *, *, #2824, .F. ) ;
#7858 = VECTOR ( 'NONE', #11008, 1000.000000000000000 ) ;
#7860 = CARTESIAN_POINT ( 'NONE',  ( -1.878215178125000939, -27.87812499938548427, 12.25316411605952283 ) ) ;
#7861 = VERTEX_POINT ( 'NONE', #6277 ) ;
#7862 = DIRECTION ( 'NONE',  ( 0.000000000000000000, -0.000000000000000000, 1.000000000000000000 ) ) ;
#7863 = EDGE_CURVE ( 'NONE', #2607, #22740, #13870, .T. ) ;
#7864 = ORIENTED_EDGE ( 'NONE', *, *, #25119, .F. ) ;
#7865 = EDGE_CURVE ( 'NONE', #6294, #7134, #19292, .T. ) ;
#7866 = CARTESIAN_POINT ( 'NONE',  ( 2.000000000000000888, 28.52500000000000213, 12.46410161513774817 ) ) ;
#7867 = CARTESIAN_POINT ( 'NONE',  ( -20.78941499438242246, -22.67092431280570963, -6.500000000000000000 ) ) ;
#7868 = ADVANCED_BREP_SHAPE_REPRESENTATION ( '', ( #13235, #21036 ), #24374 ) ;
#7869 = CARTESIAN_POINT ( 'NONE',  ( 1.878215178125000939, -12.25316411605952283, 0.6281249993854848279 ) ) ;
#7870 = LINE ( 'NONE', #12186, #8778 ) ;
#7871 = CARTESIAN_POINT ( 'NONE',  ( 21.78337204305729458, 19.12717466509784003, 5.746835883940462963 ) ) ;
#7872 = EDGE_CURVE ( 'NONE', #20357, #421, #14433, .T. ) ;
#7873 = FACE_OUTER_BOUND ( 'NONE', #15677, .T. ) ;
#7874 = VECTOR ( 'NONE', #2394, 1000.000000000000000 ) ;
#7875 = CARTESIAN_POINT ( 'NONE',  ( 5.577813053751546416E-15, 25.33750000000000924, 12.99999999999999289 ) ) ;
#7876 = VECTOR ( 'NONE', #1429, 1000.000000000000000 ) ;
#7877 = CARTESIAN_POINT ( 'NONE',  ( 2.000000000000003997, 27.32500000000000284, 5.535898384862238508 ) ) ;
#7878 = CARTESIAN_POINT ( 'NONE',  ( -3.999999999999997335, -11.30940107675849404, 3.412499999999996980 ) ) ;
#7879 = LINE ( 'NONE', #23839, #1751 ) ;
#7880 = CARTESIAN_POINT ( 'NONE',  ( -26.50000000000000355, -0.5000000000000000000, 19.00000000000000000 ) ) ;
#7881 = ORIENTED_EDGE ( 'NONE', *, *, #7539, .T. ) ;
#7882 = ORIENTED_EDGE ( 'NONE', *, *, #10714, .F. ) ;
#7883 = CARTESIAN_POINT ( 'NONE',  ( 3.756430356250004987, 25.25312499938548427, 8.999999999999992895 ) ) ;
#7884 = VERTEX_POINT ( 'NONE', #16097 ) ;
#7885 = CARTESIAN_POINT ( 'NONE',  ( 4.000000000000003553, 29.89374999877096784, 8.999999999999992895 ) ) ;
#7886 = CARTESIAN_POINT ( 'NONE',  ( -3.999999999999996003, 29.18124999877096926, 6.690598923241487306 ) ) ;
#7887 = AXIS2_PLACEMENT_3D ( 'NONE', #5163, #13142, #5280 ) ;
#7888 = CARTESIAN_POINT ( 'NONE',  ( 1.878215178125004048, 29.37812499938548783, 5.746835883940462963 ) ) ;
#7889 = CARTESIAN_POINT ( 'NONE',  ( -30.24338421796786847, -7.248980000273999025, 1.000000000000000000 ) ) ;
#7890 = ORIENTED_EDGE ( 'NONE', *, *, #7327, .T. ) ;
#7891 = ORIENTED_EDGE ( 'NONE', *, *, #13499, .T. ) ;
#7892 = CIRCLE ( 'NONE', #9555, 26.00000000000000355 ) ;
#7893 = CARTESIAN_POINT ( 'NONE',  ( -3.834746474454188013E-15, -25.56250000000000000, 4.999999999999992006 ) ) ;
#7894 = CIRCLE ( 'NONE', #9153, 31.10000000000000142 ) ;
#7895 = VERTEX_POINT ( 'NONE', #16360 ) ;
#7896 = CARTESIAN_POINT ( 'NONE',  ( 3.027510705461079255, 38.86058378564762705, 4.241563202499551544 ) ) ;
#7897 = CARTESIAN_POINT ( 'NONE',  ( -28.34936733434213707, -12.78762572734027181, -2.750000000000000000 ) ) ;
#7898 = CARTESIAN_POINT ( 'NONE',  ( 3.756430356250004099, 29.22812499938548569, 6.831223922626973533 ) ) ;
#7899 = CARTESIAN_POINT ( 'NONE',  ( 1.952785157361432100, -31.03863125411925949, 1.000000000000000000 ) ) ;
#7900 = DIRECTION ( 'NONE',  ( 1.000000000000000000, 0.000000000000000000, 0.000000000000000000 ) ) ;
#7901 = CARTESIAN_POINT ( 'NONE',  ( 4.000000000000005329, 26.83750000000000213, 6.690598923241489970 ) ) ;
#7902 = EDGE_CURVE ( 'NONE', #17175, #10674, #6144, .T. ) ;
#7903 = ADVANCED_FACE ( 'NONE', ( #11357 ), #9278, .T. ) ;
#7904 = CIRCLE ( 'NONE', #19177, 31.10000000000000142 ) ;
#7905 = CARTESIAN_POINT ( 'NONE',  ( 1.878215178125000939, 26.41562499938548214, 12.25316411605952283 ) ) ;
#7906 = CARTESIAN_POINT ( 'NONE',  ( 2.000000000000003997, -5.535898384862238508, 0.07499999999999867883 ) ) ;
#7907 = AXIS2_PLACEMENT_3D ( 'NONE', #25818, #12346, #7900 ) ;
#7908 = DIRECTION ( 'NONE',  ( 0.000000000000000000, 0.000000000000000000, 1.000000000000000000 ) ) ;
#7909 = VECTOR ( 'NONE', #25804, 1000.000000000000000 ) ;
#7910 = CARTESIAN_POINT ( 'NONE',  ( 3.834746474454188013E-15, 28.65624999877096712, 4.999999999999992006 ) ) ;
#7911 = CARTESIAN_POINT ( 'NONE',  ( 20.62984034111755705, 17.80141321637130147, 12.46410161513774817 ) ) ;
#7912 = CARTESIAN_POINT ( 'NONE',  ( 21.14697593998939595, 18.49077856202994852, 5.746835883940462963 ) ) ;
#7913 = CARTESIAN_POINT ( 'NONE',  ( -3.579383266608310077, -29.78592973091716800, 10.80044967790457378 ) ) ;
#7914 =( BOUNDED_CURVE ( )  B_SPLINE_CURVE ( 2, ( #19892, #6302, #15998, #2380, #294, #429, #24353 ),
 .UNSPECIFIED., .F., .F. ) 
 B_SPLINE_CURVE_WITH_KNOTS ( ( 3, 2, 2, 3 ),
 ( 0.2000000000000003719, 0.2166666666666670071, 0.2333333333333336423, 0.2500000000000002776 ),
 .UNSPECIFIED. ) 
 CURVE ( )  GEOMETRIC_REPRESENTATION_ITEM ( )  RATIONAL_B_SPLINE_CURVE ( ( 0.9999999999999971134, 0.8660254037844415942, 1.000000000000000000, 0.8660254037844387076, 1.000000000000000000, 0.8660254037844364872, 1.000000000000002220 ) ) 
 REPRESENTATION_ITEM ( '' )  );
#7915 = CARTESIAN_POINT ( 'NONE',  ( 4.000000000000003553, 29.48124999877097352, 6.690598923241489970 ) ) ;
#7916 = CARTESIAN_POINT ( 'NONE',  ( -3.999999999999997335, 25.26249999999999929, 11.30940107675849404 ) ) ;
#7917 = CARTESIAN_POINT ( 'NONE',  ( 0.000000000000000000, 0.000000000000000000, -6.500000000000000000 ) ) ;
#7918 = CIRCLE ( 'NONE', #2904, 0.5000000000000001110 ) ;
#7919 = EDGE_LOOP ( 'NONE', ( #6516, #10690, #14412, #16645 ) ) ;
#7920 = CARTESIAN_POINT ( 'NONE',  ( -1.999999999999998224, 27.49374999877096926, 12.46410161513774639 ) ) ;
#7921 = CARTESIAN_POINT ( 'NONE',  ( 3.999999999999996003, -27.43750000000000000, 6.690598923241487306 ) ) ;
#7923 = ORIENTED_EDGE ( 'NONE', *, *, #15852, .F. ) ;
#7922 = CARTESIAN_POINT ( 'NONE',  ( 3.756430356250004099, 26.19062499938549138, 6.831223922626973533 ) ) ;
#7924 = CARTESIAN_POINT ( 'NONE',  ( -3.756430356249996994, 27.72812499938548569, 8.999999999999992895 ) ) ;
#7925 =( BOUNDED_CURVE ( )  B_SPLINE_CURVE ( 2, ( #6667, #12168, #18317, #12698, #10591, #668, #10322 ),
 .UNSPECIFIED., .F., .F. ) 
 B_SPLINE_CURVE_WITH_KNOTS ( ( 3, 2, 2, 3 ),
 ( 0.7000000000000001776, 0.7166666666666667851, 0.7333333333333333925, 0.7500000000000000000 ),
 .UNSPECIFIED. ) 
 CURVE ( )  GEOMETRIC_REPRESENTATION_ITEM ( )  RATIONAL_B_SPLINE_CURVE ( ( 0.9999999999999982236, 0.8660254037844404840, 1.000000000000000000, 0.8660254037844387076, 1.000000000000000000, 0.8660254037844387076, 1.000000000000000000 ) ) 
 REPRESENTATION_ITEM ( '' )  );
#7926 = CARTESIAN_POINT ( 'NONE',  ( -19.82388608118395013, 23.96296185032730364, -6.500000000000000000 ) ) ;
#7927 = CIRCLE ( 'NONE', #22551, 31.10000000000000142 ) ;
#7928 = EDGE_LOOP ( 'NONE', ( #15918, #13825, #1953, #18529 ) ) ;
#7929 = CARTESIAN_POINT ( 'NONE',  ( 0.000000000000000000, 0.000000000000000000, -6.500000000000000000 ) ) ;
#7930 = ORIENTED_EDGE ( 'NONE', *, *, #7229, .T. ) ;
#7931 = ORIENTED_EDGE ( 'NONE', *, *, #8670, .T. ) ;
#7932 = DIRECTION ( 'NONE',  ( 0.000000000000000000, 0.000000000000000000, 1.000000000000000000 ) ) ;
#7933 = CARTESIAN_POINT ( 'NONE',  ( 1.878215178125006934, 26.56562499938548783, 5.746835883940462963 ) ) ;
#7934 = AXIS2_PLACEMENT_3D ( 'NONE', #20218, #6753, #20744 ) ;
#7935 = EDGE_CURVE ( 'NONE', #6036, #9323, #1044, .T. ) ;
#7936 = CARTESIAN_POINT ( 'NONE',  ( -1.878215178124998497, -12.25316411605951927, 2.240624999385484095 ) ) ;
#7937 = EDGE_CURVE ( 'NONE', #337, #10048, #2887, .T. ) ;
#7938 = VECTOR ( 'NONE', #13595, 1000.000000000000000 ) ;
#7939 = CYLINDRICAL_SURFACE ( 'NONE', #14190, 0.5000000000000004441 ) ;
#7940 = CYLINDRICAL_SURFACE ( 'NONE', #8876, 6.000000000000000888 ) ;
#7941 = AXIS2_PLACEMENT_3D ( 'NONE', #9692, #15709, #21333 ) ;
#7942 = VECTOR ( 'NONE', #5401, 1000.000000000000000 ) ;
#7943 = CARTESIAN_POINT ( 'NONE',  ( 0.000000000000000000, 0.000000000000000000, 15.00000000000000178 ) ) ;
#7944 = CARTESIAN_POINT ( 'NONE',  ( -9.110428525061097460, -29.57785765677920509, -6.500000000000000000 ) ) ;
#7945 = DIRECTION ( 'NONE',  ( 1.000000000000000000, 0.000000000000000000, 0.000000000000000000 ) ) ;
#7946 = DIRECTION ( 'NONE',  ( -1.000000000000000000, 0.000000000000000000, 0.000000000000000000 ) ) ;
#7947 = CARTESIAN_POINT ( 'NONE',  ( -1.453535542772826039, -31.06601413805601908, -2.750000000000000000 ) ) ;
#7948 = CARTESIAN_POINT ( 'NONE',  ( 19.74153744638290320, 16.91311032163664407, 5.535898384862238508 ) ) ;
#7949 = ORIENTED_EDGE ( 'NONE', *, *, #22393, .T. ) ;
#7950 = FACE_OUTER_BOUND ( 'NONE', #10739, .T. ) ;
#7951 = CARTESIAN_POINT ( 'NONE',  ( 5.532151103383234236, 38.49999999999999289, 6.677220593914319657 ) ) ;
#7952 = CARTESIAN_POINT ( 'NONE',  ( -1.878215178124995832, 27.20312499938548711, 5.746835883940462963 ) ) ;
#7953 = AXIS2_PLACEMENT_3D ( 'NONE', #21710, #11634, #9166 ) ;
#7955 = EDGE_CURVE ( 'NONE', #13093, #9331, #13078, .T. ) ;
#7954 = CARTESIAN_POINT ( 'NONE',  ( -1.999999999999998224, 29.74374999877096926, 12.46410161513774639 ) ) ;
#7956 = CARTESIAN_POINT ( 'NONE',  ( -3.999999999999998224, 26.12500000000001066, 8.999999999999992895 ) ) ;
#7957 = CARTESIAN_POINT ( 'NONE',  ( 11.44867358849351113, 28.91604871112461339, -6.500000000000000000 ) ) ;
#7958 = ORIENTED_EDGE ( 'NONE', *, *, #1367, .T. ) ;
#7959 = DIRECTION ( 'NONE',  ( 1.000000000000000000, 0.000000000000000000, 0.000000000000000000 ) ) ;
#7960 = CARTESIAN_POINT ( 'NONE',  ( 4.000000000000003553, 25.84374999877096712, 8.999999999999992895 ) ) ;
#7961 = CARTESIAN_POINT ( 'NONE',  ( 2.000000000000003553, -8.999999999999992895, 6.000000000000000000 ) ) ;
#7963 = EDGE_LOOP ( 'NONE', ( #6422, #10231, #18525, #15208 ) ) ;
#7962 = CARTESIAN_POINT ( 'NONE',  ( -4.000000000000003553, -26.38750000000000284, 6.690598923241489970 ) ) ;
#7964 = CIRCLE ( 'NONE', #19640, 0.4999999999999991673 ) ;
#7965 = ORIENTED_EDGE ( 'NONE', *, *, #5662, .F. ) ;
#7966 = ORIENTED_EDGE ( 'NONE', *, *, #13529, .T. ) ;
#7967 = PRODUCT ( 'contact point', 'contact point', '', ( #1392 ) ) ;
#7968 = ORIENTED_EDGE ( 'NONE', *, *, #10435, .F. ) ;
#7969 = DIRECTION ( 'NONE',  ( 1.000000000000000000, 0.000000000000000000, 0.000000000000000000 ) ) ;
#7970 = AXIS2_PLACEMENT_3D ( 'NONE', #776, #22627, #12938 ) ;
#7971 = DIRECTION ( 'NONE',  ( 0.000000000000000000, 0.000000000000000000, 1.000000000000000000 ) ) ;
#7972 = VECTOR ( 'NONE', #8536, 1000.000000000000000 ) ;
#7973 = FACE_OUTER_BOUND ( 'NONE', #11304, .T. ) ;
#7974 = ADVANCED_FACE ( 'NONE', ( #4835 ), #7312, .T. ) ;
#7975 = CARTESIAN_POINT ( 'NONE',  ( -3.756430356250000546, 26.75312499938548783, 11.16877607737301226 ) ) ;
#7976 = CIRCLE ( 'NONE', #20490, 4.000000000000000000 ) ;
#7977 = CARTESIAN_POINT ( 'NONE',  ( -3.756430356249996994, -8.999999999999992895, 3.065624999385483385 ) ) ;
#7978 = CARTESIAN_POINT ( 'NONE',  ( 2.000000000000003997, -5.535898384862238508, 4.068749998770968546 ) ) ;
#7979 = CARTESIAN_POINT ( 'NONE',  ( -3.756430356249997882, 28.66562499938548569, 11.16877607737301226 ) ) ;
#7980 = EDGE_CURVE ( 'NONE', #11427, #6457, #18472, .T. ) ;
#7981 = LINE ( 'NONE', #14393, #5881 ) ;
#7982 = AXIS2_PLACEMENT_3D ( 'NONE', #9578, #17951, #14028 ) ;
#7983 = CARTESIAN_POINT ( 'NONE',  ( 2.000000000000000888, -12.46410161513774817, 0.8249999999999992895 ) ) ;
#7984 = CARTESIAN_POINT ( 'NONE',  ( 1.878215178125000939, 26.86562499938548498, 12.25316411605952283 ) ) ;
#7985 = DIRECTION ( 'NONE',  ( 0.000000000000000000, 0.000000000000000000, -1.000000000000000000 ) ) ;
#7986 = CARTESIAN_POINT ( 'NONE',  ( 4.000000000000001776, 25.80624999877096926, 11.30940107675849760 ) ) ;
#7987 = DIRECTION ( 'NONE',  ( 1.000000000000000000, 0.000000000000000000, 0.000000000000000000 ) ) ;
#7988 = CARTESIAN_POINT ( 'NONE',  ( -3.752267015613588906E-15, -29.55624999877096926, 4.381197846482986158 ) ) ;
#7989 = CIRCLE ( 'NONE', #15500, 0.5000000000000003331 ) ;
#7990 = CARTESIAN_POINT ( 'NONE',  ( 1.878215178125000939, 28.32812499938548711, 12.25316411605952283 ) ) ;
#7991 = AXIS2_PLACEMENT_3D ( 'NONE', #8328, #10544, #625 ) ;
#7993 = EDGE_CURVE ( 'NONE', #8636, #5294, #23255, .T. ) ;
#7992 = DIRECTION ( 'NONE',  ( 0.000000000000000000, 0.000000000000000000, 1.000000000000000000 ) ) ;
#7994 = FACE_OUTER_BOUND ( 'NONE', #2657, .T. ) ;
#7995 = FACE_OUTER_BOUND ( 'NONE', #9671, .T. ) ;
#7996 = VERTEX_POINT ( 'NONE', #25099 ) ;
#7998 = VERTEX_POINT ( 'NONE', #3004 ) ;
#7997 = CARTESIAN_POINT ( 'NONE',  ( 26.25859848311259981, -16.66421332384692278, -6.500000000000000000 ) ) ;
#7999 = VECTOR ( 'NONE', #22720, 1000.000000000000000 ) ;
#8000 = ORIENTED_EDGE ( 'NONE', *, *, #12007, .F. ) ;
#8001 = FACE_OUTER_BOUND ( 'NONE', #1594, .T. ) ;
#8002 = ORIENTED_EDGE ( 'NONE', *, *, #5950, .T. ) ;
#8003 = CARTESIAN_POINT ( 'NONE',  ( -2.672651547586948120E-15, -26.82812499938548356, 13.33755215474602984 ) ) ;
#8004 = ORIENTED_EDGE ( 'NONE', *, *, #11799, .F. ) ;
#8005 = LINE ( 'NONE', #289, #23020 ) ;
#8006 = AXIS2_PLACEMENT_3D ( 'NONE', #20972, #11021, #19002 ) ;
#8007 = ORIENTED_EDGE ( 'NONE', *, *, #4324, .T. ) ;
#8008 = CARTESIAN_POINT ( 'NONE',  ( -1.999999999999995781, 29.19999999999999929, 5.535898384862237620 ) ) ;
#8009 = CARTESIAN_POINT ( 'NONE',  ( 2.672651547586948120E-15, 27.39062499938548356, 13.33755215474603162 ) ) ;
#8010 = CIRCLE ( 'NONE', #17623, 0.5000000000000001110 ) ;
#8011 = AXIS2_PLACEMENT_3D ( 'NONE', #18988, #7083, #1073 ) ;
#8012 = CARTESIAN_POINT ( 'NONE',  ( 3.756430356250002323, -11.16877607737301226, 1.115624999385483429 ) ) ;
#8013 = CARTESIAN_POINT ( 'NONE',  ( -16.66421332384701515, -26.25859848311253941, 1.000000000000000000 ) ) ;
#8014 = CARTESIAN_POINT ( 'NONE',  ( 21.06742642710591440, 18.41122904914646341, 5.746835883940462963 ) ) ;
#8015 = DIRECTION ( 'NONE',  ( 0.000000000000000000, 0.000000000000000000, 1.000000000000000000 ) ) ;
#8016 = EDGE_CURVE ( 'NONE', #6983, #14487, #18957, .T. ) ;
#8017 = FACE_BOUND ( 'NONE', #22744, .T. ) ;
#8018 = CARTESIAN_POINT ( 'NONE',  ( 4.000000000000001776, 27.21250000000000213, 11.30940107675849760 ) ) ;
#8019 = CYLINDRICAL_SURFACE ( 'NONE', #15896, 6.000000000000000888 ) ;
#8020 = EDGE_CURVE ( 'NONE', #5409, #9972, #15155, .T. ) ;
#8021 = CARTESIAN_POINT ( 'NONE',  ( 1.071796769724492338, 25.80759618943233491, 12.99999999999999467 ) ) ;
#8022 = CARTESIAN_POINT ( 'NONE',  ( 5.706339097770919189, 31.50000000000000000, 7.145898033750285983 ) ) ;
#8023 = VECTOR ( 'NONE', #14665, 1000.000000000000000 ) ;
#8024 = ORIENTED_EDGE ( 'NONE', *, *, #14498, .F. ) ;
#8025 = ORIENTED_EDGE ( 'NONE', *, *, #4105, .F. ) ;
#8026 = CARTESIAN_POINT ( 'NONE',  ( 2.000000000000003553, 29.06874999877097210, 5.535898384862238508 ) ) ;
#8027 = AXIS2_PLACEMENT_3D ( 'NONE', #22751, #21047, #3122 ) ;
#8028 = CIRCLE ( 'NONE', #4691, 31.10000000000000142 ) ;
#8029 = ORIENTED_EDGE ( 'NONE', *, *, #1365, .F. ) ;
#8030 = CARTESIAN_POINT ( 'NONE',  ( -26.00000000000000355, 0.000000000000000000, 19.59999999999999787 ) ) ;
#8031 = CARTESIAN_POINT ( 'NONE',  ( 3.735045420075836212E-15, 25.81562499938548783, 4.662447845253954171 ) ) ;
#8032 = CARTESIAN_POINT ( 'NONE',  ( 15.57844627214710975, 21.23530052163942372, 6.690598923241487306 ) ) ;
#8033 = AXIS2_PLACEMENT_3D ( 'NONE', #21960, #5875, #25634 ) ;
#8034 = CARTESIAN_POINT ( 'NONE',  ( 18.67203843983824996, 18.67203843983818246, 4.999999999999991118 ) ) ;
#8035 = EDGE_CURVE ( 'NONE', #16822, #7170, #5529, .T. ) ;
#8036 = ORIENTED_EDGE ( 'NONE', *, *, #2436, .F. ) ;
#8037 = VECTOR ( 'NONE', #349, 1000.000000000000000 ) ;
#8038 = CARTESIAN_POINT ( 'NONE',  ( -1.999999999999993117, 25.99374999877097281, 5.535898384862237620 ) ) ;
#8039 = ORIENTED_EDGE ( 'NONE', *, *, #21096, .F. ) ;
#8040 = DIRECTION ( 'NONE',  ( 1.000000000000000000, 0.000000000000000000, 0.000000000000000000 ) ) ;
#8041 = CARTESIAN_POINT ( 'NONE',  ( 1.878215178125004048, 27.01562499938548711, 5.746835883940462963 ) ) ;
#8042 = CARTESIAN_POINT ( 'NONE',  ( 4.000000000000003553, 29.05000000000000071, 8.999999999999992895 ) ) ;
#8043 = CIRCLE ( 'NONE', #8468, 0.5000000000000000000 ) ;
#8044 = CARTESIAN_POINT ( 'NONE',  ( 5.577813053751546416E-15, 25.33750000000000213, 12.99999999999999289 ) ) ;
#8045 = CARTESIAN_POINT ( 'NONE',  ( 2.000000000000003997, 29.51874999877096784, 5.535898384862238508 ) ) ;
#8046 = ADVANCED_FACE ( 'NONE', ( #18828 ), #13324, .T. ) ;
#8047 = CARTESIAN_POINT ( 'NONE',  ( -3.999999999999999556, 27.51250000000000639, 11.30940107675849404 ) ) ;
#8048 = AXIS2_PLACEMENT_3D ( 'NONE', #22668, #10738, #19927 ) ;
#8049 = CARTESIAN_POINT ( 'NONE',  ( 3.756430356250004099, 25.17812499938548498, 6.831223922626973533 ) ) ;
#8050 = DIRECTION ( 'NONE',  ( -0.000000000000000000, 0.000000000000000000, 1.000000000000000000 ) ) ;
#8051 = CARTESIAN_POINT ( 'NONE',  ( 4.000000000000003553, -8.999999999999992895, 2.700000000000001066 ) ) ;
#8052 = DIRECTION ( 'NONE',  ( 1.000000000000000000, 0.000000000000000000, 0.000000000000000000 ) ) ;
#8053 = CARTESIAN_POINT ( 'NONE',  ( 17.32411613907045478, 20.15254326381657535, 5.535898384862237620 ) ) ;
#8054 = CYLINDRICAL_SURFACE ( 'NONE', #12640, 4.000000000000000000 ) ;
#8055 = ADVANCED_FACE ( 'NONE', ( #16881 ), #5221, .F. ) ;
#8056 = DIRECTION ( 'NONE',  ( 0.000000000000000000, 0.000000000000000000, -1.000000000000000000 ) ) ;
#8057 = CARTESIAN_POINT ( 'NONE',  ( -1.999999999999998224, 29.29374999877096997, 12.46410161513774639 ) ) ;
#8058 = CARTESIAN_POINT ( 'NONE',  ( -1.999999999999998224, 25.30000000000000426, 12.46410161513774639 ) ) ;
#8059 = CARTESIAN_POINT ( 'NONE',  ( 19.10065816080342671, 21.75685553876272493, 5.746835883940462963 ) ) ;
#8060 = ORIENTED_EDGE ( 'NONE', *, *, #16115, .F. ) ;
#8061 = CARTESIAN_POINT ( 'NONE',  ( 4.000000000000001776, 28.50624999877096855, 11.30940107675849760 ) ) ;
#8062 = CARTESIAN_POINT ( 'NONE',  ( -2.620986760973688460E-15, -27.58750000000000213, 13.61880215351699874 ) ) ;
#8063 = EDGE_CURVE ( 'NONE', #6029, #13686, #943, .T. ) ;
#8065 = ORIENTED_EDGE ( 'NONE', *, *, #15086, .T. ) ;
#8064 = CARTESIAN_POINT ( 'NONE',  ( 3.756430356250000546, 26.56562499938549138, 11.16877607737301403 ) ) ;
#8066 = CARTESIAN_POINT ( 'NONE',  ( 2.672651547586948120E-15, 27.39062499938548356, 13.33755215474603162 ) ) ;
#8067 = ADVANCED_FACE ( 'NONE', ( #13199 ), #1157, .F. ) ;
#8068 = CIRCLE ( 'NONE', #12656, 0.4999999999999997780 ) ;
#8069 = DIRECTION ( 'NONE',  ( 0.000000000000000000, 0.000000000000000000, 1.000000000000000000 ) ) ;
#8070 = PLANE ( 'NONE',  #18833 ) ;
#8071 = VERTEX_POINT ( 'NONE', #19199 ) ;
#8072 = VERTEX_POINT ( 'NONE', #14783 ) ;
#8073 =( NAMED_UNIT ( * ) PLANE_ANGLE_UNIT ( ) SI_UNIT ( $, .RADIAN. ) );
#8074 = CARTESIAN_POINT ( 'NONE',  ( 6.009258394948636914E-15, 27.95312499938548356, 4.662447845253954171 ) ) ;
#8075 = CARTESIAN_POINT ( 'NONE',  ( -1.859271017917182139E-15, -28.88124999877096499, 12.99999999999999289 ) ) ;
#8076 = CARTESIAN_POINT ( 'NONE',  ( 1.878215178125004048, -5.746835883940462963, 2.465624999385483740 ) ) ;
#8077 = CIRCLE ( 'NONE', #6811, 0.5000000000000007772 ) ;
#8078 = CARTESIAN_POINT ( 'NONE',  ( 3.469446951953614189E-15, 30.00000000000000355, 4.999999999999992006 ) ) ;
#8079 =( BOUNDED_CURVE ( )  B_SPLINE_CURVE ( 2, ( #3628, #7559, #7688, #7179, #11480, #5216, #15671, #13579, #13072 ),
 .UNSPECIFIED., .F., .F. ) 
 B_SPLINE_CURVE_WITH_KNOTS ( ( 3, 2, 2, 2, 3 ),
 ( 0.7750000000000000222, 0.7833333333333333259, 0.8000000000000000444, 0.8166666666666666519, 0.8250000000000000666 ),
 .UNSPECIFIED. ) 
 CURVE ( )  GEOMETRIC_REPRESENTATION_ITEM ( )  RATIONAL_B_SPLINE_CURVE ( ( 0.9330127018922194093, 0.9330127018922194093, 1.000000000000000000, 0.8660254037844387076, 1.000000000000000000, 0.8660254037844387076, 1.000000000000000000, 0.9330127018922189652, 0.9330127018922194093 ) ) 
 REPRESENTATION_ITEM ( '' )  );
#8080 = FACE_BOUND ( 'NONE', #9536, .T. ) ;
#8081 = CARTESIAN_POINT ( 'NONE',  ( -5.706339097770935176, 31.50000000000000000, 7.645898033750358813 ) ) ;
#8082 = CARTESIAN_POINT ( 'NONE',  ( 0.000000000000000000, 0.000000000000000000, 4.999999999999993783 ) ) ;
#8083 = DIRECTION ( 'NONE',  ( 0.000000000000000000, 0.000000000000000000, 1.000000000000000000 ) ) ;
#8084 = CARTESIAN_POINT ( 'NONE',  ( 4.000000000000003553, 25.44999999999999929, 8.999999999999992895 ) ) ;
#8085 = LINE ( 'NONE', #7947, #6617 ) ;
#8086 = CARTESIAN_POINT ( 'NONE',  ( 16.53304042674895058, 22.18989467624125922, 6.690598923241487306 ) ) ;
#8087 = ORIENTED_EDGE ( 'NONE', *, *, #12336, .F. ) ;
#8088 = DIRECTION ( 'NONE',  ( 0.000000000000000000, 0.000000000000000000, 1.000000000000000000 ) ) ;
#8089 = CARTESIAN_POINT ( 'NONE',  ( 5.326315416280042569, 38.74360394679613506, 6.816580744743770737 ) ) ;
#8090 =( BOUNDED_CURVE ( )  B_SPLINE_CURVE ( 2, ( #6118, #14102, #5069, #25209, #18797, #5315, #19310 ),
 .UNSPECIFIED., .F., .F. ) 
 B_SPLINE_CURVE_WITH_KNOTS ( ( 3, 2, 2, 3 ),
 ( 0.6500000000000002442, 0.6666666666666668517, 0.6833333333333335702, 0.7000000000000001776 ),
 .UNSPECIFIED. ) 
 CURVE ( )  GEOMETRIC_REPRESENTATION_ITEM ( )  RATIONAL_B_SPLINE_CURVE ( ( 0.9999999999999982236, 0.8660254037844404840, 1.000000000000000000, 0.8660254037844387076, 1.000000000000000000, 0.8660254037844369313, 1.000000000000001776 ) ) 
 REPRESENTATION_ITEM ( '' )  );
#8091 = CARTESIAN_POINT ( 'NONE',  ( -1.878215178124998497, 27.80312499938548498, 12.25316411605951927 ) ) ;
#8092 = CYLINDRICAL_SURFACE ( 'NONE', #22073, 0.5000000000000004441 ) ;
#8093 =( GEOMETRIC_REPRESENTATION_CONTEXT ( 3 ) GLOBAL_UNCERTAINTY_ASSIGNED_CONTEXT ( ( #4713 ) ) GLOBAL_UNIT_ASSIGNED_CONTEXT ( ( #3407, #17407, #5364 ) ) REPRESENTATION_CONTEXT ( 'NONE', 'WORKASPACE' ) );
#8094 = CARTESIAN_POINT ( 'NONE',  ( 7.901901826148023498E-15, 26.23750000000000426, 12.99999999999999112 ) ) ;
#8095 = CARTESIAN_POINT ( 'NONE',  ( 0.000000000000000000, 0.000000000000000000, 1.000000000000000000 ) ) ;
#8096 = ORIENTED_EDGE ( 'NONE', *, *, #136, .F. ) ;
#8097 = LINE ( 'NONE', #511, #78 ) ;
#8098 = DIRECTION ( 'NONE',  ( 0.000000000000000000, -0.000000000000000000, 1.000000000000000000 ) ) ;
#8099 = DIRECTION ( 'NONE',  ( 0.000000000000000000, 0.000000000000000000, -1.000000000000000000 ) ) ;
#8100 = ADVANCED_FACE ( 'NONE', ( #24846 ), #22758, .F. ) ;
#8102 = ORIENTED_EDGE ( 'NONE', *, *, #13932, .F. ) ;
#8101 = DIRECTION ( 'NONE',  ( -0.7071067811865487940, -0.7071067811865463515, 0.000000000000000000 ) ) ;
#8103 = EDGE_CURVE ( 'NONE', #7056, #20899, #25732, .T. ) ;
#8104 = AXIS2_PLACEMENT_3D ( 'NONE', #8741, #6786, #14771 ) ;
#8105 = EDGE_LOOP ( 'NONE', ( #9943, #19178, #22501, #11916 ) ) ;
#8106 = ORIENTED_EDGE ( 'NONE', *, *, #1716, .F. ) ;
#8107 = ORIENTED_EDGE ( 'NONE', *, *, #22188, .F. ) ;
#8108 = DIRECTION ( 'NONE',  ( 1.000000000000000000, 0.000000000000000000, 0.000000000000000000 ) ) ;
#8109 = EDGE_CURVE ( 'NONE', #7744, #16500, #3858, .T. ) ;
#8110 = DIRECTION ( 'NONE',  ( -0.000000000000000000, -0.000000000000000000, 1.000000000000000000 ) ) ;
#8111 = CARTESIAN_POINT ( 'NONE',  ( 27.25313774936419620, 14.98253926456328244, 1.000000000000000000 ) ) ;
#8112 = CARTESIAN_POINT ( 'NONE',  ( -3.756430356249997882, 26.26562499938548711, 8.999999999999992895 ) ) ;
#8113 =( GEOMETRIC_REPRESENTATION_CONTEXT ( 3 ) GLOBAL_UNCERTAINTY_ASSIGNED_CONTEXT ( ( #1292 ) ) GLOBAL_UNIT_ASSIGNED_CONTEXT ( ( #12896, #7004, #2573 ) ) REPRESENTATION_CONTEXT ( 'NONE', 'WORKASPACE' ) );
#8114 = CARTESIAN_POINT ( 'NONE',  ( 1.878215178125004048, -5.746835883940462963, 4.265624999385483562 ) ) ;
#8115 = CARTESIAN_POINT ( 'NONE',  ( 3.735045420075836212E-15, -4.662447845253954171, 0.3656249993854837066 ) ) ;
#8116 = CARTESIAN_POINT ( 'NONE',  ( 3.756430356250002323, 26.45312499938548356, 11.16877607737301226 ) ) ;
#8117 = DIRECTION ( 'NONE',  ( 0.000000000000000000, 0.000000000000000000, 1.000000000000000000 ) ) ;
#8118 = CARTESIAN_POINT ( 'NONE',  ( -27.64012133169333651, -13.24173596767349359, -6.500000000000000000 ) ) ;
#8119 = CARTESIAN_POINT ( 'NONE',  ( 1.878215178125004048, 27.01562499938548711, 5.746835883940462963 ) ) ;
#8120 = DIRECTION ( 'NONE',  ( 0.000000000000000000, 0.000000000000000000, 1.000000000000000000 ) ) ;
#8121 = CARTESIAN_POINT ( 'NONE',  ( 1.071796769724487230, -25.52634618820330559, 4.999999999999992006 ) ) ;
#8122 = DIRECTION ( 'NONE',  ( 1.000000000000000000, 0.000000000000000000, 0.000000000000000000 ) ) ;
#8123 = CARTESIAN_POINT ( 'NONE',  ( 1.999999999999995781, -28.24374999877096570, 5.535898384862237620 ) ) ;
#8124 = CARTESIAN_POINT ( 'NONE',  ( 1.878215178125004048, 28.92812499938548854, 5.746835883940462963 ) ) ;
#8125 = CARTESIAN_POINT ( 'NONE',  ( 5.577813053751546416E-15, 28.20624999877096784, 4.999999999999992006 ) ) ;
#8126 = FACE_OUTER_BOUND ( 'NONE', #17519, .T. ) ;
#8127 = ORIENTED_EDGE ( 'NONE', *, *, #20142, .T. ) ;
#8128 = CARTESIAN_POINT ( 'NONE',  ( 1.859271017917182139E-15, 28.48749999999999716, 12.99999999999999289 ) ) ;
#8130 = ORIENTED_EDGE ( 'NONE', *, *, #16516, .T. ) ;
#8129 = CARTESIAN_POINT ( 'NONE',  ( 8.217531866530997320, -29.99470236596036088, -2.750000000000000000 ) ) ;
#8131 = EDGE_CURVE ( 'NONE', #16191, #14853, #10954, .T. ) ;
#8132 = ADVANCED_FACE ( 'NONE', ( #1939 ), #9658, .F. ) ;
#8133 = VERTEX_POINT ( 'NONE', #11740 ) ;
#8134 = ORIENTED_EDGE ( 'NONE', *, *, #7937, .T. ) ;
#8135 = ORIENTED_EDGE ( 'NONE', *, *, #642, .T. ) ;
#8136 = EDGE_LOOP ( 'NONE', ( #25861, #25686, #4068, #133 ) ) ;
#8137 = DIRECTION ( 'NONE',  ( 0.000000000000000000, 0.000000000000000000, 1.000000000000000000 ) ) ;
#8138 = ORIENTED_EDGE ( 'NONE', *, *, #3482, .T. ) ;
#8139 = DIRECTION ( 'NONE',  ( 0.000000000000000000, -0.000000000000000000, 1.000000000000000000 ) ) ;
#8140 = CARTESIAN_POINT ( 'NONE',  ( 3.756430356250003211, 27.09062499938548640, 6.831223922626973533 ) ) ;
#8141 = ADVANCED_FACE ( 'NONE', ( #5855 ), #23438, .F. ) ;
#8142 = CARTESIAN_POINT ( 'NONE',  ( 3.756430356250003655, -8.999999999999992895, 2.953124999385485339 ) ) ;
#8143 = DIRECTION ( 'NONE',  ( 1.000000000000000000, 0.000000000000000000, 0.000000000000000000 ) ) ;
#8144 = CARTESIAN_POINT ( 'NONE',  ( 20.74922837557196331, 18.09303099761251588, 5.746835883940462963 ) ) ;
#8145 = DIRECTION ( 'NONE',  ( 1.000000000000000000, 0.000000000000000000, 0.000000000000000000 ) ) ;
#8146 = CYLINDRICAL_SURFACE ( 'NONE', #10442, 0.5000000000000004441 ) ;
#8147 = CARTESIAN_POINT ( 'NONE',  ( 3.735045420075836212E-15, -4.662447845253954171, 1.603124999385479921 ) ) ;
#8148 = CARTESIAN_POINT ( 'NONE',  ( 4.000000000000003553, 27.25000000000000000, 8.999999999999992895 ) ) ;
#8149 = CARTESIAN_POINT ( 'NONE',  ( -17.08421000182741878, 25.98730014090460116, -2.750000000000000000 ) ) ;
#8150 = CARTESIAN_POINT ( 'NONE',  ( -3.999999999999996447, -8.999999999999992895, 3.374999999999999556 ) ) ;
#8151 = CARTESIAN_POINT ( 'NONE',  ( 4.000000000000003553, 25.90000000000000213, 8.999999999999992895 ) ) ;
#8152 = CARTESIAN_POINT ( 'NONE',  ( 4.648177544792954952E-15, 28.26250000000000284, 4.999999999999992006 ) ) ;
#8153 = ORIENTED_EDGE ( 'NONE', *, *, #7384, .F. ) ;
#8154 = EDGE_LOOP ( 'NONE', ( #21210, #23240, #16505, #6807 ) ) ;
#8155 = CARTESIAN_POINT ( 'NONE',  ( -1.999999999999996669, 29.74374999877097636, 12.46410161513774639 ) ) ;
#8156 = ORIENTED_EDGE ( 'NONE', *, *, #25063, .F. ) ;
#8157 = CARTESIAN_POINT ( 'NONE',  ( -30.54913349766228592, -5.827558883615738594, -6.500000000000000000 ) ) ;
#8158 = CARTESIAN_POINT ( 'NONE',  ( -3.756430356249995661, 25.89062499938548356, 6.831223922626973533 ) ) ;
#8159 = CARTESIAN_POINT ( 'NONE',  ( 16.96614333022570875, 19.79457045497182577, 5.535898384862237620 ) ) ;
#8160 = DIRECTION ( 'NONE',  ( 0.000000000000000000, 0.000000000000000000, 1.000000000000000000 ) ) ;
#8161 = ORIENTED_EDGE ( 'NONE', *, *, #7141, .F. ) ;
#8162 = SHAPE_REPRESENTATION ( 'revolution counter', ( #21036 ), #582 ) ;
#8163 = FACE_OUTER_BOUND ( 'NONE', #23370, .T. ) ;
#8164 = VERTEX_POINT ( 'NONE', #12845 ) ;
#8165 = ADVANCED_FACE ( 'NONE', ( #24610 ), #8054, .F. ) ;
#8166 = AXIS2_PLACEMENT_3D ( 'NONE', #2123, #8139, #22256 ) ;
#8167 = CYLINDRICAL_SURFACE ( 'NONE', #16843, 0.5000000000000004441 ) ;
#8168 = CARTESIAN_POINT ( 'NONE',  ( 1.878215178125004048, 27.91562499938548569, 5.746835883940462963 ) ) ;
#8169 = CARTESIAN_POINT ( 'NONE',  ( -3.756430356249996549, 29.37812499938548427, 6.831223922626973533 ) ) ;
#8170 = CARTESIAN_POINT ( 'NONE',  ( -29.57785765677936851, -9.610428525060582317, -6.500000000000000000 ) ) ;
#8171 = CARTESIAN_POINT ( 'NONE',  ( -1.071796769724489451, 26.48259618943233562, 4.999999999999992895 ) ) ;
#8172 = CARTESIAN_POINT ( 'NONE',  ( 2.000000000000005329, 28.67500000000000426, 5.535898384862238508 ) ) ;
#8173 = AXIS2_PLACEMENT_3D ( 'NONE', #7450, #21071, #12603 ) ;
#8174 = CARTESIAN_POINT ( 'NONE',  ( -4.000000000000003553, -29.69687499938548569, 8.999999999999992895 ) ) ;
#8175 = CARTESIAN_POINT ( 'NONE',  ( -1.071796769724487230, 27.38259618943233420, 4.999999999999992006 ) ) ;
#8176 = DIRECTION ( 'NONE',  ( 0.000000000000000000, 1.000000000000000000, -0.000000000000000000 ) ) ;
#8177 = PRODUCT ( 'bezel', 'bezel', '', ( #21014 ) ) ;
#8178 = FACE_OUTER_BOUND ( 'NONE', #11884, .T. ) ;
#8179 = LINE ( 'NONE', #16156, #7172 ) ;
#8180 = CARTESIAN_POINT ( 'NONE',  ( 21.00669330961039449, 19.49094378175826847, 4.999999999999992895 ) ) ;
#8181 = CARTESIAN_POINT ( 'NONE',  ( 3.756430356249996105, -25.77812499938548285, 6.831223922626973533 ) ) ;
#8182 = DIRECTION ( 'NONE',  ( 0.000000000000000000, 0.000000000000000000, 1.000000000000000000 ) ) ;
#8183 = ORIENTED_EDGE ( 'NONE', *, *, #14768, .T. ) ;
#8184 = CARTESIAN_POINT ( 'NONE',  ( -3.999999999999996003, 28.73124999877096641, 6.690598923241487306 ) ) ;
#8185 = CARTESIAN_POINT ( 'NONE',  ( 3.999999999999996447, -28.82499999999999929, 8.999999999999992895 ) ) ;
#8187 = ORIENTED_EDGE ( 'NONE', *, *, #23256, .F. ) ;
#8186 = CARTESIAN_POINT ( 'NONE',  ( -1.878215178124996498, 27.20312499938549067, 5.746835883940462963 ) ) ;
#8188 = CARTESIAN_POINT ( 'NONE',  ( -3.756430356249997438, 28.66562499938548569, 11.16877607737301048 ) ) ;
#8189 =( BOUNDED_CURVE ( )  B_SPLINE_CURVE ( 2, ( #12801, #6519, #20775, #4431, #526, #2853, #10820 ),
 .UNSPECIFIED., .F., .F. ) 
 B_SPLINE_CURVE_WITH_KNOTS ( ( 3, 2, 2, 3 ),
 ( 0.3999999999999999667, 0.4166666666666665741, 0.4333333333333332371, 0.4499999999999998446 ),
 .UNSPECIFIED. ) 
 CURVE ( )  GEOMETRIC_REPRESENTATION_ITEM ( )  RATIONAL_B_SPLINE_CURVE ( ( 1.000000000000000444, 0.8660254037844382635, 1.000000000000000000, 0.8660254037844387076, 1.000000000000000000, 0.8660254037844400399, 0.9999999999999986677 ) ) 
 REPRESENTATION_ITEM ( '' )  );
#8190 = DIRECTION ( 'NONE',  ( -0.7071067811865487940, -0.7071067811865463515, -0.000000000000000000 ) ) ;
#8191 = LINE ( 'NONE', #14348, #9618 ) ;
#8192 = ORIENTED_EDGE ( 'NONE', *, *, #19852, .T. ) ;
#8193 = ORIENTED_EDGE ( 'NONE', *, *, #16100, .T. ) ;
#8194 = CARTESIAN_POINT ( 'NONE',  ( 21.28941499438209206, -22.67092431280601872, -6.500000000000000000 ) ) ;
#8195 = CARTESIAN_POINT ( 'NONE',  ( 3.756430356250002323, 28.25312499938548783, 11.16877607737301226 ) ) ;
#8196 = CARTESIAN_POINT ( 'NONE',  ( 3.959305671612554781E-15, 30.00000000000000355, 12.99999999999999289 ) ) ;
#8197 = ADVANCED_FACE ( 'NONE', ( #21909 ), #10131, .F. ) ;
#8198 = CARTESIAN_POINT ( 'NONE',  ( 1.878215178125000939, -12.25316411605952283, 2.315624999385482941 ) ) ;
#8199 = EDGE_CURVE ( 'NONE', #20048, #13450, #4292, .T. ) ;
#8200 = CARTESIAN_POINT ( 'NONE',  ( -3.999999999999998224, 28.31874999877097210, 8.999999999999992895 ) ) ;
#8201 =( NAMED_UNIT ( * ) SI_UNIT ( $, .STERADIAN. ) SOLID_ANGLE_UNIT ( ) );
#8202 = ADVANCED_FACE ( 'NONE', ( #4112 ), #4250, .F. ) ;
#8203 = CARTESIAN_POINT ( 'NONE',  ( 30.54913349766219710, -5.827558883616158703, -6.500000000000000000 ) ) ;
#8204 = CARTESIAN_POINT ( 'NONE',  ( -17.78012134629613783, -25.16042852506070560, 1.000000000000000000 ) ) ;
#8205 = FACE_OUTER_BOUND ( 'NONE', #25006, .T. ) ;
#8206 = CARTESIAN_POINT ( 'NONE',  ( 21.10271800016700183, 15.44586375067455464, 8.999999999999992895 ) ) ;
#8207 = CARTESIAN_POINT ( 'NONE',  ( 4.000000000000001776, 25.41250000000000142, 11.30940107675849760 ) ) ;
#8208 = CARTESIAN_POINT ( 'NONE',  ( 20.32496430686003208, 17.66876692890059530, 12.25316411605952283 ) ) ;
#8209 = CARTESIAN_POINT ( 'NONE',  ( 16.85123847828289811, 22.50809272777520675, 6.690598923241487306 ) ) ;
#8210 = ORIENTED_EDGE ( 'NONE', *, *, #546, .T. ) ;
#8211 = CARTESIAN_POINT ( 'NONE',  ( 0.000000000000000000, 0.000000000000000000, 1.000000000000000000 ) ) ;
#8212 = DIRECTION ( 'NONE',  ( 1.000000000000000000, 0.000000000000000000, 0.000000000000000000 ) ) ;
#8213 = CARTESIAN_POINT ( 'NONE',  ( 3.756430356250004099, 25.17812499938548498, 6.831223922626973533 ) ) ;
#8215 = EDGE_LOOP ( 'NONE', ( #9562, #12849 ) ) ;
#8214 = CARTESIAN_POINT ( 'NONE',  ( -3.595210675795415867, 29.78396494222454294, 7.227341970420264161 ) ) ;
#8216 = CARTESIAN_POINT ( 'NONE',  ( -1.071796769724488785, 29.31115380933864145, 12.99999999999999289 ) ) ;
#8217 = FACE_OUTER_BOUND ( 'NONE', #22251, .T. ) ;
#8218 = ORIENTED_EDGE ( 'NONE', *, *, #6345, .T. ) ;
#8219 = DIRECTION ( 'NONE',  ( -0.000000000000000000, 1.000000000000000000, -0.000000000000000000 ) ) ;
#8220 = FACE_OUTER_BOUND ( 'NONE', #20418, .T. ) ;
#8221 = CARTESIAN_POINT ( 'NONE',  ( -3.735045420075836212E-15, -27.05312499938548498, 4.662447845253954171 ) ) ;
#8223 = ORIENTED_EDGE ( 'NONE', *, *, #18466, .T. ) ;
#8222 = DIRECTION ( 'NONE',  ( 0.7289686274214101092, -0.6845471059286901694, 0.000000000000000000 ) ) ;
#8224 = ORIENTED_EDGE ( 'NONE', *, *, #13962, .T. ) ;
#8225 = ORIENTED_EDGE ( 'NONE', *, *, #8423, .F. ) ;
#8226 = ORIENTED_EDGE ( 'NONE', *, *, #3234, .F. ) ;
#8227 = DIRECTION ( 'NONE',  ( 0.000000000000000000, 0.000000000000000000, 1.000000000000000000 ) ) ;
#8228 = FACE_OUTER_BOUND ( 'NONE', #15082, .T. ) ;
#8229 = CARTESIAN_POINT ( 'NONE',  ( -3.999999999999995559, 26.48124999877096641, 6.690598923241487306 ) ) ;
#8230 = CARTESIAN_POINT ( 'NONE',  ( -3.756430356249994773, 28.06562499938548783, 8.999999999999992895 ) ) ;
#8231 = CARTESIAN_POINT ( 'NONE',  ( -7.901901826148023498E-15, 28.71250000000000568, 4.999999999999992006 ) ) ;
#8232 = CARTESIAN_POINT ( 'NONE',  ( -1.878215178124998497, -12.25316411605951927, 0.5531249993854860936 ) ) ;
#8233 = EDGE_CURVE ( 'NONE', #24375, #4269, #19319, .T. ) ;
#8234 =( BOUNDED_CURVE ( )  B_SPLINE_CURVE ( 2, ( #7811, #15931, #21813, #23903, #20096, #19955, #15672, #5851, #3896 ),
 .UNSPECIFIED., .F., .T. ) 
 B_SPLINE_CURVE_WITH_KNOTS ( ( 3, 2, 2, 2, 3 ),
 ( 0.8750000000000000000, 0.8833333333333333037, 0.9000000000000000222, 0.9166666666666666297, 0.9250000000000000444 ),
 .UNSPECIFIED. ) 
 CURVE ( )  GEOMETRIC_REPRESENTATION_ITEM ( )  RATIONAL_B_SPLINE_CURVE ( ( 0.9330127018922194093, 0.9330127018922194093, 1.000000000000000000, 0.8660254037844387076, 1.000000000000000000, 0.8660254037844387076, 1.000000000000000000, 0.9330127018922189652, 0.9330127018922194093 ) ) 
 REPRESENTATION_ITEM ( '' )  );
#8235 = CARTESIAN_POINT ( 'NONE',  ( -3.756430356249996994, 26.71562499938548285, 8.999999999999992895 ) ) ;
#8236 = ADVANCED_FACE ( 'NONE', ( #10870 ), #326, .F. ) ;
#8237 = DIRECTION ( 'NONE',  ( -1.000000000000000000, 0.000000000000000000, 0.000000000000000000 ) ) ;
#8238 = CARTESIAN_POINT ( 'NONE',  ( 2.620986760973688460E-15, -13.61880215351699874, 1.631249998770966991 ) ) ;
#8239 = CARTESIAN_POINT ( 'NONE',  ( 1.878215178125004048, 26.56562499938548427, 5.746835883940462963 ) ) ;
#8240 = DIRECTION ( 'NONE',  ( 0.000000000000000000, 0.000000000000000000, 1.000000000000000000 ) ) ;
#8241 = FACE_OUTER_BOUND ( 'NONE', #20969, .T. ) ;
#8242 = CARTESIAN_POINT ( 'NONE',  ( -3.999999999999996447, -8.999999999999992895, 3.824999999999998401 ) ) ;
#8243 = CARTESIAN_POINT ( 'NONE',  ( -3.752267015613588906E-15, -28.20624999877096784, 4.381197846482986158 ) ) ;
#8244 = EDGE_CURVE ( 'NONE', #16170, #6260, #10967, .T. ) ;
#8245 = CARTESIAN_POINT ( 'NONE',  ( 2.672651547586948120E-15, 29.64062499938548356, 13.33755215474602984 ) ) ;
#8246 = CARTESIAN_POINT ( 'NONE',  ( -3.469446951953614189E-15, -30.00000000000000355, 4.999999999999992006 ) ) ;
#8247 = DIRECTION ( 'NONE',  ( 0.000000000000000000, -0.000000000000000000, 1.000000000000000000 ) ) ;
#8248 = CARTESIAN_POINT ( 'NONE',  ( 3.974466138550253103, -29.73560671006806899, 8.477544402765669673 ) ) ;
#8249 = ORIENTED_EDGE ( 'NONE', *, *, #23882, .T. ) ;
#8250 = CARTESIAN_POINT ( 'NONE',  ( 13.24173596767359662, -28.14012133169329388, -6.500000000000000000 ) ) ;
#8252 = VERTEX_POINT ( 'NONE', #18133 ) ;
#8251 = FACE_OUTER_BOUND ( 'NONE', #17584, .T. ) ;
#8253 = ORIENTED_EDGE ( 'NONE', *, *, #12763, .T. ) ;
#8254 = EDGE_CURVE ( 'NONE', #22773, #24763, #25592, .T. ) ;
#8255 = ORIENTED_EDGE ( 'NONE', *, *, #10394, .F. ) ;
#8256 = VERTEX_POINT ( 'NONE', #20194 ) ;
#8257 = ORIENTED_EDGE ( 'NONE', *, *, #8562, .T. ) ;
#8258 = CARTESIAN_POINT ( 'NONE',  ( -29.99470236596038220, -8.217531866530892515, -2.750000000000000000 ) ) ;
#8259 = VERTEX_POINT ( 'NONE', #2030 ) ;
#8260 = CARTESIAN_POINT ( 'NONE',  ( 2.000000000000000888, 29.42500000000000071, 12.46410161513774817 ) ) ;
#8261 = CARTESIAN_POINT ( 'NONE',  ( 3.756430356250003655, 26.60312499938548569, 8.999999999999992895 ) ) ;
#8262 = ADVANCED_FACE ( 'NONE', ( #8178 ), #17994, .F. ) ;
#8263 = CARTESIAN_POINT ( 'NONE',  ( -3.756430356249997882, -11.16877607737301226, 2.765624999385486227 ) ) ;
#8264 = CARTESIAN_POINT ( 'NONE',  ( 21.06969990136081705, 15.75730514544200211, 8.999999999999992895 ) ) ;
#8265 = CARTESIAN_POINT ( 'NONE',  ( 15.41874213889396117, -27.00874656207311020, -2.750000000000000000 ) ) ;
#8266 = EDGE_CURVE ( 'NONE', #11238, #32, #14064, .T. ) ;
#8267 = DIRECTION ( 'NONE',  ( 0.000000000000000000, 0.000000000000000000, 1.000000000000000000 ) ) ;
#8268 = AXIS2_PLACEMENT_3D ( 'NONE', #2655, #4473, #16641 ) ;
#8269 = CARTESIAN_POINT ( 'NONE',  ( -1.878215178124995832, -5.746835883940462963, 1.190624999385481830 ) ) ;
#8270 = CARTESIAN_POINT ( 'NONE',  ( 2.000000000000000888, 29.42500000000000071, 12.46410161513774817 ) ) ;
#8271 = DIRECTION ( 'NONE',  ( -0.8660254037844397068, 0.000000000000000000, 0.4999999999999983347 ) ) ;
#8272 = CARTESIAN_POINT ( 'NONE',  ( -1.878215178124995832, -5.746835883940462963, 1.303124999385483429 ) ) ;
#8273 = DIRECTION ( 'NONE',  ( 0.000000000000000000, 1.000000000000000000, 0.000000000000000000 ) ) ;
#8274 = CARTESIAN_POINT ( 'NONE',  ( -1.071796769724498999, -28.05759618943233491, 12.99999999999998757 ) ) ;
#8275 = AXIS2_PLACEMENT_3D ( 'NONE', #16680, #725, #8834 ) ;
#8276 = EDGE_LOOP ( 'NONE', ( #13151, #17485, #6007, #14110 ) ) ;
#8277 = ORIENTED_EDGE ( 'NONE', *, *, #20905, .F. ) ;
#8278 = CARTESIAN_POINT ( 'NONE',  ( -3.756430356249998326, 27.24062499938548854, 6.831223922626973533 ) ) ;
#8279 = EDGE_CURVE ( 'NONE', #14017, #12396, #4756, .T. ) ;
#8280 = VERTEX_POINT ( 'NONE', #83 ) ;
#8281 = DIRECTION ( 'NONE',  ( 0.3681245526846732008, -0.9297764858882532346, 0.000000000000000000 ) ) ;
#8282 = ORIENTED_EDGE ( 'NONE', *, *, #10638, .F. ) ;
#8283 = CARTESIAN_POINT ( 'NONE',  ( 21.44743255599544440, 15.79057830650299366, 6.690598923241489970 ) ) ;
#8284 = ORIENTED_EDGE ( 'NONE', *, *, #900, .T. ) ;
#8285 = AXIS2_PLACEMENT_3D ( 'NONE', #20139, #10451, #16494 ) ;
#8286 = CARTESIAN_POINT ( 'NONE',  ( 1.952785157361650370, 31.03863125411924528, -6.500000000000000000 ) ) ;
#8287 = ORIENTED_EDGE ( 'NONE', *, *, #23723, .F. ) ;
#8288 = CARTESIAN_POINT ( 'NONE',  ( 1.626862140677534194E-14, 28.43124999877096570, 12.99999999999999289 ) ) ;
#8289 = CARTESIAN_POINT ( 'NONE',  ( 1.878215178125000939, 28.21562499938548640, 12.25316411605952283 ) ) ;
#8290 = DIRECTION ( 'NONE',  ( 0.8660254037844395958, -0.4999999999999982236, 0.000000000000000000 ) ) ;
#8291 = AXIS2_PLACEMENT_3D ( 'NONE', #18875, #21091, #16920 ) ;
#8292 = CARTESIAN_POINT ( 'NONE',  ( -25.99307600111999150, -0.5999999999999996447, 19.00000000000000000 ) ) ;
#8293 = DIRECTION ( 'NONE',  ( 0.000000000000000000, 0.000000000000000000, 1.000000000000000000 ) ) ;
#8294 = CARTESIAN_POINT ( 'NONE',  ( -1.999999999999998224, 28.30000000000000426, 5.535898384862237620 ) ) ;
#8295 = CARTESIAN_POINT ( 'NONE',  ( -3.756430356249996994, 28.06562499938548427, 8.999999999999992895 ) ) ;
#8296 = EDGE_CURVE ( 'NONE', #21691, #9505, #23999, .T. ) ;
#8297 = DIRECTION ( 'NONE',  ( 1.000000000000000000, 0.000000000000000000, 0.000000000000000000 ) ) ;
#8298 = CIRCLE ( 'NONE', #8285, 31.10000000000000142 ) ;
#8299 = CIRCLE ( 'NONE', #23754, 0.4999999999999987232 ) ;
#8300 = CARTESIAN_POINT ( 'NONE',  ( 22.00869856443133088, 19.18027143968506465, 5.535898384862238508 ) ) ;
#8301 = CARTESIAN_POINT ( 'NONE',  ( -1.999999999999995781, -5.535898384862237620, 4.593749998770966236 ) ) ;
#8302 = DIRECTION ( 'NONE',  ( 0.000000000000000000, 1.000000000000000000, 0.000000000000000000 ) ) ;
#8304 = FACE_OUTER_BOUND ( 'NONE', #3461, .T. ) ;
#8303 = VECTOR ( 'NONE', #8695, 1000.000000000000000 ) ;
#8305 = DIRECTION ( 'NONE',  ( -0.9921147013144768767, 0.1253332335643120576, 0.000000000000000000 ) ) ;
#8306 = AXIS2_PLACEMENT_3D ( 'NONE', #4414, #6503, #16329 ) ;
#8307 = ORIENTED_EDGE ( 'NONE', *, *, #16598, .F. ) ;
#8308 = CARTESIAN_POINT ( 'NONE',  ( -3.999999999999996447, 27.41874999877096641, 8.999999999999992895 ) ) ;
#8309 = CARTESIAN_POINT ( 'NONE',  ( 22.37551020630278842, 16.71865595681033412, 8.999999999999992895 ) ) ;
#8311 = ORIENTED_EDGE ( 'NONE', *, *, #5790, .F. ) ;
#8310 = CARTESIAN_POINT ( 'NONE',  ( 1.878215178125003382, 28.02812499938548996, 5.746835883940462963 ) ) ;
#8312 = ORIENTED_EDGE ( 'NONE', *, *, #12498, .T. ) ;
#8313 = CARTESIAN_POINT ( 'NONE',  ( 3.959305671612554781E-15, 40.00000000000000000, 12.99999999999999289 ) ) ;
#8314 = DIRECTION ( 'NONE',  ( 0.000000000000000000, 0.000000000000000000, 1.000000000000000000 ) ) ;
#8315 = ORIENTED_EDGE ( 'NONE', *, *, #19124, .F. ) ;
#8316 = ORIENTED_EDGE ( 'NONE', *, *, #24116, .T. ) ;
#8317 = CARTESIAN_POINT ( 'NONE',  ( 3.756430356249996994, -26.37812499938548783, 8.999999999999992895 ) ) ;
#8318 = CARTESIAN_POINT ( 'NONE',  ( 1.878215178125001605, 28.66562499938549280, 12.25316411605952283 ) ) ;
#8319 = CARTESIAN_POINT ( 'NONE',  ( 1.071796769724494558, 28.18615380933863435, 4.999999999999992895 ) ) ;
#8320 = VECTOR ( 'NONE', #11429, 1000.000000000000000 ) ;
#8321 = CARTESIAN_POINT ( 'NONE',  ( -31.10000000000000142, 3.257552089140643357E-13, -6.500000000000000000 ) ) ;
#8322 = AXIS2_PLACEMENT_3D ( 'NONE', #975, #4771, #21102 ) ;
#8323 = VECTOR ( 'NONE', #12875, 1000.000000000000000 ) ;
#8324 = DIRECTION ( 'NONE',  ( -0.8660254037844397068, -0.4999999999999983347, 0.000000000000000000 ) ) ;
#8325 = CARTESIAN_POINT ( 'NONE',  ( 4.000000000000003553, -8.999999999999992895, 4.049999999999998046 ) ) ;
#8326 = LINE ( 'NONE', #13697, #15524 ) ;
#8327 = EDGE_CURVE ( 'NONE', #8668, #22605, #24758, .T. ) ;
#8328 = CARTESIAN_POINT ( 'NONE',  ( 0.000000000000000000, 0.000000000000000000, -6.500000000000000000 ) ) ;
#8329 = AXIS2_PLACEMENT_3D ( 'NONE', #8685, #7609, #3551 ) ;
#8330 = CARTESIAN_POINT ( 'NONE',  ( -9.110428525060477511, 29.57785765677940404, 1.000000000000000000 ) ) ;
#8331 = DIRECTION ( 'NONE',  ( -0.000000000000000000, -0.000000000000000000, -1.000000000000000000 ) ) ;
#8332 = CARTESIAN_POINT ( 'NONE',  ( 21.04318339706631846, 15.73078864114750530, 11.16877607737301226 ) ) ;
#8333 = CARTESIAN_POINT ( 'NONE',  ( 21.22646168687465007, 18.39803456212839450, 12.46410161513774817 ) ) ;
#8334 = ORIENTED_EDGE ( 'NONE', *, *, #15730, .F. ) ;
#8335 = CARTESIAN_POINT ( 'NONE',  ( 3.999999999999995559, -26.98750000000000071, 6.690598923241487306 ) ) ;
#8336 = DIRECTION ( 'NONE',  ( 1.000000000000000000, 0.000000000000000000, 0.000000000000000000 ) ) ;
#8337 = CARTESIAN_POINT ( 'NONE',  ( -3.756430356249996994, 26.26562499938548711, 8.999999999999992895 ) ) ;
#8340 = EDGE_CURVE ( 'NONE', #13787, #1315, #14329, .T. ) ;
#8339 = ORIENTED_EDGE ( 'NONE', *, *, #1391, .F. ) ;
#8338 = DIRECTION ( 'NONE',  ( 0.000000000000000000, 0.000000000000000000, 1.000000000000000000 ) ) ;
#8341 = CARTESIAN_POINT ( 'NONE',  ( 20.77801835412136100, 15.46562359820254784, 6.831223922626973533 ) ) ;
#8342 = DIRECTION ( 'NONE',  ( 0.9659258262890673130, -0.2588190451025242922, 0.000000000000000000 ) ) ;
#8343 = ORIENTED_EDGE ( 'NONE', *, *, #15631, .F. ) ;
#8344 = DIRECTION ( 'NONE',  ( 0.000000000000000000, 0.000000000000000000, 1.000000000000000000 ) ) ;
#8345 = CARTESIAN_POINT ( 'NONE',  ( 2.000000000000003997, 25.91874999877096997, 5.535898384862238508 ) ) ;
#8346 = CARTESIAN_POINT ( 'NONE',  ( -3.756430356250004099, -26.07812499938548356, 6.831223922626973533 ) ) ;
#8348 = ORIENTED_EDGE ( 'NONE', *, *, #15959, .F. ) ;
#8347 = DIRECTION ( 'NONE',  ( -0.000000000000000000, -1.000000000000000000, -0.000000000000000000 ) ) ;
#8349 = EDGE_CURVE ( 'NONE', #15624, #20629, #5143, .T. ) ;
#8350 = CIRCLE ( 'NONE', #425, 0.5000000000000006661 ) ;
#8351 = VERTEX_POINT ( 'NONE', #5139 ) ;
#8352 = ORIENTED_EDGE ( 'NONE', *, *, #14474, .T. ) ;
#8353 = EDGE_CURVE ( 'NONE', #13915, #7056, #21602, .T. ) ;
#8354 = ORIENTED_EDGE ( 'NONE', *, *, #19672, .F. ) ;
#8355 = DIRECTION ( 'NONE',  ( 1.000000000000000000, 0.000000000000000000, 0.000000000000000000 ) ) ;
#8356 = CARTESIAN_POINT ( 'NONE',  ( 2.003086131649545506E-15, 25.59062499938548996, 13.33755215474602984 ) ) ;
#8357 = CIRCLE ( 'NONE', #22561, 1.000000000000000000 ) ;
#8358 = AXIS2_PLACEMENT_3D ( 'NONE', #19104, #5249, #22661 ) ;
#8359 = AXIS2_PLACEMENT_3D ( 'NONE', #17238, #9380, #11070 ) ;
#8360 = CARTESIAN_POINT ( 'NONE',  ( -1.071796769724489895, 28.91740381056767362, 12.99999999999999289 ) ) ;
#8361 = CARTESIAN_POINT ( 'NONE',  ( 1.878215178125004048, -5.746835883940462963, 2.578124999385485339 ) ) ;
#8362 = CARTESIAN_POINT ( 'NONE',  ( -3.756430356249996994, 27.16562499938548214, 8.999999999999992895 ) ) ;
#8363 = VECTOR ( 'NONE', #18984, 1000.000000000000000 ) ;
#8364 = DIRECTION ( 'NONE',  ( 0.9980267284282724471, 0.06279051952930156388, 0.000000000000000000 ) ) ;
#8365 = CARTESIAN_POINT ( 'NONE',  ( -3.999999999999996447, -8.999999999999992895, 0.6749999999999984901 ) ) ;
#8366 = CARTESIAN_POINT ( 'NONE',  ( 3.735045420075836212E-15, 26.15312499938548285, 4.662447845253954171 ) ) ;
#8367 = CARTESIAN_POINT ( 'NONE',  ( -5.827558883616271501, -30.54913349766217934, -6.500000000000000000 ) ) ;
#8368 = DIRECTION ( 'NONE',  ( -0.4817536741017063306, 0.8763066800438685799, 0.000000000000000000 ) ) ;
#8369 = CARTESIAN_POINT ( 'NONE',  ( -1.999999999999998224, 28.84374999877096712, 12.46410161513774639 ) ) ;
#8370 = CARTESIAN_POINT ( 'NONE',  ( -3.756430356250004099, -25.74062499938548143, 6.831223922626973533 ) ) ;
#8371 = CYLINDRICAL_SURFACE ( 'NONE', #2729, 0.5000000000000004441 ) ;
#8372 = DIRECTION ( 'NONE',  ( -0.000000000000000000, -0.000000000000000000, -1.000000000000000000 ) ) ;
#8373 = EDGE_CURVE ( 'NONE', #7266, #1051, #13116, .T. ) ;
#8374 = VECTOR ( 'NONE', #24617, 1000.000000000000000 ) ;
#8375 = CARTESIAN_POINT ( 'NONE',  ( 1.999999999999998224, -25.30000000000000426, 12.46410161513774639 ) ) ;
#8376 = ORIENTED_EDGE ( 'NONE', *, *, #9576, .F. ) ;
#8377 = FACE_OUTER_BOUND ( 'NONE', #19731, .T. ) ;
#8379 = VERTEX_POINT ( 'NONE', #19492 ) ;
#8378 = LINE ( 'NONE', #8763, #16261 ) ;
#8380 = AXIS2_PLACEMENT_3D ( 'NONE', #5719, #15674, #1428 ) ;
#8381 = CIRCLE ( 'NONE', #6729, 31.10000000000000142 ) ;
#8382 = ORIENTED_EDGE ( 'NONE', *, *, #20992, .T. ) ;
#8383 = ORIENTED_EDGE ( 'NONE', *, *, #18594, .T. ) ;
#8384 = ORIENTED_EDGE ( 'NONE', *, *, #6167, .F. ) ;
#8385 = EDGE_CURVE ( 'NONE', #11726, #23620, #23136, .T. ) ;
#8386 = ORIENTED_EDGE ( 'NONE', *, *, #2089, .F. ) ;
#8387 = VERTEX_POINT ( 'NONE', #15325 ) ;
#8388 = CARTESIAN_POINT ( 'NONE',  ( -1.999999999999995781, -5.535898384862237620, 2.793749998770966858 ) ) ;
#8390 = EDGE_CURVE ( 'NONE', #15232, #1313, #22293, .T. ) ;
#8389 = AXIS2_PLACEMENT_3D ( 'NONE', #3895, #9896, #18270 ) ;
#8391 = ORIENTED_EDGE ( 'NONE', *, *, #22992, .F. ) ;
#8392 = CYLINDRICAL_SURFACE ( 'NONE', #19424, 3.000000000000000444 ) ;
#8393 = CARTESIAN_POINT ( 'NONE',  ( 3.756430356250003211, 27.54062499938547859, 6.831223922626973533 ) ) ;
#8394 =( BOUNDED_CURVE ( )  B_SPLINE_CURVE ( 2, ( #8552, #17971, #10232, #18229, #312, #8283, #12335, #16265, #8034 ),
 .UNSPECIFIED., .F., .F. ) 
 B_SPLINE_CURVE_WITH_KNOTS ( ( 3, 2, 2, 2, 3 ),
 ( 0.1750000000000000167, 0.1833333333333333204, 0.2000000000000000111, 0.2166666666666666741, 0.2250000000000000056 ),
 .UNSPECIFIED. ) 
 CURVE ( )  GEOMETRIC_REPRESENTATION_ITEM ( )  RATIONAL_B_SPLINE_CURVE ( ( 0.9330127018922194093, 0.9330127018922196314, 1.000000000000000000, 0.8660254037844387076, 1.000000000000000000, 0.8660254037844387076, 1.000000000000000000, 0.9330127018922194093, 0.9330127018922194093 ) ) 
 REPRESENTATION_ITEM ( '' )  );
#8395 = AXIS2_PLACEMENT_3D ( 'NONE', #12176, #8137, #13754 ) ;
#8396 = CARTESIAN_POINT ( 'NONE',  ( 3.735045420075836212E-15, -4.662447845253954171, 2.165624999385483029 ) ) ;
#8397 = CARTESIAN_POINT ( 'NONE',  ( 0.000000000000000000, 0.000000000000000000, -6.500000000000000000 ) ) ;
#8398 = PRODUCT_DEFINITION_SHAPE ( 'NONE', 'NONE',  #22284 ) ;
#8399 = CARTESIAN_POINT ( 'NONE',  ( 22.31597560320210505, 17.00358084728328478, 11.16877607737301226 ) ) ;
#8400 = VECTOR ( 'NONE', #5475, 1000.000000000000000 ) ;
#8401 = DIRECTION ( 'NONE',  ( 0.000000000000000000, 0.000000000000000000, 1.000000000000000000 ) ) ;
#8402 = AXIS2_PLACEMENT_3D ( 'NONE', #6957, #4752, #12722 ) ;
#8403 = FACE_OUTER_BOUND ( 'NONE', #18704, .T. ) ;
#8404 = CARTESIAN_POINT ( 'NONE',  ( -3.756430356249996994, -8.999999999999992895, 2.615624999385480987 ) ) ;
#8405 = CARTESIAN_POINT ( 'NONE',  ( 2.000000000000000888, -12.46410161513774817, 4.424999999999998046 ) ) ;
#8406 = DIRECTION ( 'NONE',  ( 0.000000000000000000, 0.000000000000000000, 1.000000000000000000 ) ) ;
#8407 = CARTESIAN_POINT ( 'NONE',  ( 3.756430356250002323, 28.25312499938548427, 11.16877607737301403 ) ) ;
#8408 = AXIS2_PLACEMENT_3D ( 'NONE', #25314, #5570, #21016 ) ;
#8409 = CARTESIAN_POINT ( 'NONE',  ( 1.878215178125004048, -5.746835883940462963, 1.228124999385484584 ) ) ;
#8410 = CARTESIAN_POINT ( 'NONE',  ( 2.000000000000003997, 25.97500000000000142, 5.535898384862238508 ) ) ;
#8411 = CARTESIAN_POINT ( 'NONE',  ( -4.000000000000001776, -28.11250000000000071, 11.30940107675849760 ) ) ;
#8412 = VERTEX_POINT ( 'NONE', #3164 ) ;
#8413 = ORIENTED_EDGE ( 'NONE', *, *, #1839, .T. ) ;
#8414 = CARTESIAN_POINT ( 'NONE',  ( -3.756430356249994329, 26.86562499938548498, 11.16877607737301226 ) ) ;
#8415 = AXIS2_PLACEMENT_3D ( 'NONE', #25282, #21363, #21219 ) ;
#8416 = EDGE_LOOP ( 'NONE', ( #5325, #19115, #15079, #20768 ) ) ;
#8417 = CARTESIAN_POINT ( 'NONE',  ( -0.7500000000000000000, -2.999999999999999556, 18.19999999999999929 ) ) ;
#8418 = EDGE_CURVE ( 'NONE', #4092, #18554, #5565, .T. ) ;
#8419 = ORIENTED_EDGE ( 'NONE', *, *, #3267, .T. ) ;
#8420 = CARTESIAN_POINT ( 'NONE',  ( -3.999999999999997335, 26.16250000000000142, 11.30940107675849404 ) ) ;
#8421 = VERTEX_POINT ( 'NONE', #22916 ) ;
#8422 = DIRECTION ( 'NONE',  ( -0.5358267949790012086, -0.8443279255020122998, 0.000000000000000000 ) ) ;
#8423 = EDGE_CURVE ( 'NONE', #5410, #21566, #3047, .T. ) ;
#8424 = AXIS2_PLACEMENT_3D ( 'NONE', #6372, #16698, #16455 ) ;
#8425 = DIRECTION ( 'NONE',  ( 0.06279051952932236669, 0.9980267284282710039, 0.000000000000000000 ) ) ;
#8426 = EDGE_LOOP ( 'NONE', ( #20466, #13566, #8210, #10955 ) ) ;
#8427 = CARTESIAN_POINT ( 'NONE',  ( 4.000000000000003553, 28.54374999877096997, 8.999999999999992895 ) ) ;
#8428 = CARTESIAN_POINT ( 'NONE',  ( 3.756430356250004099, 27.42812499938548143, 6.831223922626973533 ) ) ;
#8429 = CARTESIAN_POINT ( 'NONE',  ( 0.000000000000000000, 0.000000000000000000, -6.500000000000000000 ) ) ;
#8430 = CIRCLE ( 'NONE', #18458, 0.4999999999999983902 ) ;
#8431 = DIRECTION ( 'NONE',  ( 1.000000000000000000, 0.000000000000000000, 0.000000000000000000 ) ) ;
#8432 = LINE ( 'NONE', #20055, #25434 ) ;
#8433 = CARTESIAN_POINT ( 'NONE',  ( 2.000000000000000000, 28.97500000000000853, 12.46410161513774817 ) ) ;
#8434 = CIRCLE ( 'NONE', #18873, 0.5000000000000003331 ) ;
#8435 = CARTESIAN_POINT ( 'NONE',  ( -1.878215178124995832, 27.99062499938548143, 5.746835883940462963 ) ) ;
#8436 = VECTOR ( 'NONE', #6140, 1000.000000000000000 ) ;
#8437 = CIRCLE ( 'NONE', #24306, 31.10000000000000142 ) ;
#8438 = DIRECTION ( 'NONE',  ( 0.000000000000000000, 1.000000000000000000, 0.000000000000000000 ) ) ;
#8439 = CARTESIAN_POINT ( 'NONE',  ( 17.84560739019553921, 23.50246163968784430, 6.690598923241487306 ) ) ;
#8440 = CARTESIAN_POINT ( 'NONE',  ( -1.071796769724493448, 29.18259618943233136, 4.999999999999995559 ) ) ;
#8441 = CARTESIAN_POINT ( 'NONE',  ( -3.834746474454188013E-15, -27.75624999877096855, 4.999999999999992006 ) ) ;
#8442 = CIRCLE ( 'NONE', #20556, 0.5000000000000011102 ) ;
#8443 = LINE ( 'NONE', #87, #9571 ) ;
#8444 = CARTESIAN_POINT ( 'NONE',  ( 5.220798168720365062, 38.91217497027906802, 10.99271487579059325 ) ) ;
#8445 = ORIENTED_EDGE ( 'NONE', *, *, #13635, .F. ) ;
#8446 = CARTESIAN_POINT ( 'NONE',  ( 4.000000000000001776, 29.40624999877096357, 11.30940107675849760 ) ) ;
#8447 = CARTESIAN_POINT ( 'NONE',  ( 3.999999999999996447, -28.37500000000000000, 8.999999999999992895 ) ) ;
#8449 = ORIENTED_EDGE ( 'NONE', *, *, #15924, .F. ) ;
#8448 = CARTESIAN_POINT ( 'NONE',  ( 3.756430356250002323, 27.91562499938548925, 11.16877607737301403 ) ) ;
#8450 = EDGE_CURVE ( 'NONE', #284, #9659, #13897, .T. ) ;
#8451 = ORIENTED_EDGE ( 'NONE', *, *, #6324, .T. ) ;
#8452 = CARTESIAN_POINT ( 'NONE',  ( 1.057460391440397258E-14, -29.10624999877096641, 4.999999999999992006 ) ) ;
#8453 = CIRCLE ( 'NONE', #15547, 26.00000000000000711 ) ;
#8454 = CARTESIAN_POINT ( 'NONE',  ( 3.874318223440419207, 38.57128445889050283, 4.512312944482766319 ) ) ;
#8455 = CARTESIAN_POINT ( 'NONE',  ( 5.577813053751546416E-15, 25.73124999877097352, 12.99999999999999289 ) ) ;
#8456 = VERTEX_POINT ( 'NONE', #7089 ) ;
#8457 = EDGE_LOOP ( 'NONE', ( #21614, #21990, #18999, #1597 ) ) ;
#8458 = CARTESIAN_POINT ( 'NONE',  ( 1.878215178124995832, -27.65312499938548640, 5.746835883940462963 ) ) ;
#8459 = CARTESIAN_POINT ( 'NONE',  ( -3.756430356250000546, 28.55312499938549564, 11.16877607737301226 ) ) ;
#8460 = CARTESIAN_POINT ( 'NONE',  ( -1.626862140677534194E-14, -28.03750000000000497, 12.99999999999999289 ) ) ;
#8461 = EDGE_CURVE ( 'NONE', #12953, #14487, #17668, .T. ) ;
#8462 = CARTESIAN_POINT ( 'NONE',  ( 3.469446951953614189E-15, 30.00000000000000355, 4.999999999999992006 ) ) ;
#8463 = ADVANCED_FACE ( 'NONE', ( #25001 ), #17302, .T. ) ;
#8464 = FACE_OUTER_BOUND ( 'NONE', #2047, .T. ) ;
#8465 = CARTESIAN_POINT ( 'NONE',  ( 0.000000000000000000, 10.00000000000000000, -2.999999999999999112 ) ) ;
#8466 = DIRECTION ( 'NONE',  ( 0.000000000000000000, -0.000000000000000000, 1.000000000000000000 ) ) ;
#8467 = LINE ( 'NONE', #18541, #16348 ) ;
#8468 = AXIS2_PLACEMENT_3D ( 'NONE', #6129, #21959, #12144 ) ;
#8469 = LINE ( 'NONE', #6758, #13830 ) ;
#8470 = DIRECTION ( 'NONE',  ( 1.387778780781445044E-14, 1.000000000000000000, 0.000000000000000000 ) ) ;
#8471 = CARTESIAN_POINT ( 'NONE',  ( 17.61573392031167273, 20.27193129827097806, 12.25316411605951927 ) ) ;
#8472 = CARTESIAN_POINT ( 'NONE',  ( 23.62178590814407642, 17.96493165865162567, 11.30940107675849760 ) ) ;
#8473 = CARTESIAN_POINT ( 'NONE',  ( -1.071796769724488563, 28.46740381056766722, 12.99999999999999289 ) ) ;
#8474 = CARTESIAN_POINT ( 'NONE',  ( 26.49999999999999645, 0.5000000000000000000, 19.50000000000000000 ) ) ;
#8475 = CARTESIAN_POINT ( 'NONE',  ( 1.878215178125004048, 25.21562499938548285, 5.746835883940462963 ) ) ;
#8476 = AXIS2_PLACEMENT_3D ( 'NONE', #22030, #24754, #23873 ) ;
#8478 = VERTEX_POINT ( 'NONE', #13368 ) ;
#8477 = CARTESIAN_POINT ( 'NONE',  ( 0.000000000000000000, 0.000000000000000000, 1.000000000000000000 ) ) ;
#8479 = LINE ( 'NONE', #16582, #16675 ) ;
#8480 = DIRECTION ( 'NONE',  ( -0.9685831611286319642, -0.2486898871648515197, 0.000000000000000000 ) ) ;
#8481 = ORIENTED_EDGE ( 'NONE', *, *, #18899, .T. ) ;
#8482 = FACE_OUTER_BOUND ( 'NONE', #3773, .T. ) ;
#8483 = CARTESIAN_POINT ( 'NONE',  ( 2.620986760973688460E-15, 25.73124999877096997, 13.61880215351699874 ) ) ;
#8484 = CARTESIAN_POINT ( 'NONE',  ( -3.735045420075836212E-15, -27.50312499938548783, 4.662447845253954171 ) ) ;
#8486 = ORIENTED_EDGE ( 'NONE', *, *, #12733, .T. ) ;
#8485 = FACE_OUTER_BOUND ( 'NONE', #23389, .T. ) ;
#8487 = DIRECTION ( 'NONE',  ( -0.000000000000000000, -1.000000000000000000, -0.000000000000000000 ) ) ;
#8488 = CIRCLE ( 'NONE', #16861, 31.10000000000000142 ) ;
#8489 = ORIENTED_EDGE ( 'NONE', *, *, #2510, .T. ) ;
#8490 = CARTESIAN_POINT ( 'NONE',  ( -3.756430356250002323, -25.55312499938548143, 11.16877607737301226 ) ) ;
#8491 = VERTEX_POINT ( 'NONE', #21341 ) ;
#8492 = VERTEX_POINT ( 'NONE', #25522 ) ;
#8493 = CARTESIAN_POINT ( 'NONE',  ( 3.110308778861349932, 38.49999999999999289, 14.13088484572963033 ) ) ;
#8494 = CARTESIAN_POINT ( 'NONE',  ( 1.859271017917182139E-15, 27.08124999877096784, 12.99999999999999289 ) ) ;
#8495=STYLED_ITEM('',(#25907),#4848);
#8496 = EDGE_CURVE ( 'NONE', #25184, #6156, #13623, .T. ) ;
#8497 = LINE ( 'NONE', #22867, #21044 ) ;
#8498 = EDGE_CURVE ( 'NONE', #14582, #25359, #21590, .T. ) ;
#8499 = ADVANCED_FACE ( 'NONE', ( #9559 ), #3669, .T. ) ;
#8500 = CARTESIAN_POINT ( 'NONE',  ( -3.756430356249996994, -8.999999999999992895, 1.378124999385485605 ) ) ;
#8501 = SURFACE_STYLE_FILL_AREA ( #20252 ) ;
#8502 = CARTESIAN_POINT ( 'NONE',  ( -4.000000000000003553, -29.50000000000000355, 8.999999999999992895 ) ) ;
#8503 = CARTESIAN_POINT ( 'NONE',  ( 3.756430356250003655, 25.59062499938548285, 8.999999999999992895 ) ) ;
#8504 = LINE ( 'NONE', #16486, #15508 ) ;
#8505 = LINE ( 'NONE', #12685, #22171 ) ;
#8506 = PRESENTATION_LAYER_ASSIGNMENT (  '', '', ( #18128 ) ) ;
#8507 = CARTESIAN_POINT ( 'NONE',  ( 1.878215178125000939, 25.51562499938548356, 12.25316411605952283 ) ) ;
#8508 = CARTESIAN_POINT ( 'NONE',  ( 0.000000000000000000, 0.000000000000000000, 1.000000000000000000 ) ) ;
#8510 = ADVANCED_FACE ( 'NONE', ( #15592 ), #11907, .T. ) ;
#8509 = CARTESIAN_POINT ( 'NONE',  ( 22.54985889724113335, 19.78820606519062508, 12.50294890599016639 ) ) ;
#8511 = DIRECTION ( 'NONE',  ( 1.000000000000000000, 0.000000000000000000, 0.000000000000000000 ) ) ;
#8512 = CARTESIAN_POINT ( 'NONE',  ( 1.878215178124995832, -27.65312499938548640, 5.746835883940462963 ) ) ;
#8513 = DIRECTION ( 'NONE',  ( 1.000000000000000000, 0.000000000000000000, 0.000000000000000000 ) ) ;
#8514 = DIRECTION ( 'NONE',  ( 0.000000000000000000, 0.000000000000000000, 1.000000000000000000 ) ) ;
#8515 = CARTESIAN_POINT ( 'NONE',  ( 19.03001124868299243, 19.03001124868293559, 4.999999999999991118 ) ) ;
#8516 = CARTESIAN_POINT ( 'NONE',  ( 25.99519186311192342, -0.5000000000000000000, 20.00000000000000000 ) ) ;
#8517 = ORIENTED_EDGE ( 'NONE', *, *, #4897, .F. ) ;
#8518 = CYLINDRICAL_SURFACE ( 'NONE', #1240, 6.000000000000000888 ) ;
#8520 = ORIENTED_EDGE ( 'NONE', *, *, #12071, .F. ) ;
#8519 = CARTESIAN_POINT ( 'NONE',  ( 31.00322564728514507, 2.451530025009026836, -2.750000000000000000 ) ) ;
#8521 = ORIENTED_EDGE ( 'NONE', *, *, #7238, .T. ) ;
#8522 = ORIENTED_EDGE ( 'NONE', *, *, #19673, .F. ) ;
#8523 = ORIENTED_EDGE ( 'NONE', *, *, #13932, .T. ) ;
#8524 = ADVANCED_FACE ( 'NONE', ( #25771 ), #17805, .F. ) ;
#8525 = EDGE_LOOP ( 'NONE', ( #19459, #14079, #5235, #18117 ) ) ;
#8526 = ORIENTED_EDGE ( 'NONE', *, *, #604, .F. ) ;
#8527 = CARTESIAN_POINT ( 'NONE',  ( 10.08469938919499320, 29.41953157733090762, -2.750000000000000000 ) ) ;
#8528 = VERTEX_POINT ( 'NONE', #1728 ) ;
#8529 = DIRECTION ( 'NONE',  ( 0.000000000000000000, 0.000000000000000000, 1.000000000000000000 ) ) ;
#8530 = CARTESIAN_POINT ( 'NONE',  ( 3.756430356250003655, 28.85312499938548569, 8.999999999999992895 ) ) ;
#8531 = ADVANCED_FACE ( 'NONE', ( #8126 ), #11787, .T. ) ;
#8532 = CARTESIAN_POINT ( 'NONE',  ( 3.756430356250004099, -6.831223922626973533, 2.090624999385480631 ) ) ;
#8533 = CARTESIAN_POINT ( 'NONE',  ( -3.999999999999996447, -8.999999999999992895, 0.6187499987709670357 ) ) ;
#8534 = CARTESIAN_POINT ( 'NONE',  ( 15.88988766691455368, 21.20228242283322828, 6.831223922626973533 ) ) ;
#8535 = ADVANCED_FACE ( 'NONE', ( #19622 ), #9701, .T. ) ;
#8536 = DIRECTION ( 'NONE',  ( -0.000000000000000000, -0.000000000000000000, -1.000000000000000000 ) ) ;
#8537 = CARTESIAN_POINT ( 'NONE',  ( 0.000000000000000000, 0.000000000000000000, -6.500000000000000000 ) ) ;
#8538 = CARTESIAN_POINT ( 'NONE',  ( -3.756430356249997882, -11.16877607737301226, 2.653124999385483296 ) ) ;
#8540 = ADVANCED_FACE ( 'NONE', ( #7995 ), #10074, .F. ) ;
#8539 = CARTESIAN_POINT ( 'NONE',  ( 4.000000000000001776, -11.30940107675849760, 3.112500000000001155 ) ) ;
#8541 = CARTESIAN_POINT ( 'NONE',  ( -3.999999999999996447, 28.80624999877097281, 11.30940107675849404 ) ) ;
#8542 = CARTESIAN_POINT ( 'NONE',  ( 22.32573188046920265, 21.65113613650335367, -6.500000000000000000 ) ) ;
#8543 = CARTESIAN_POINT ( 'NONE',  ( 2.672651547586948120E-15, -13.33755215474603162, 1.490624999385481209 ) ) ;
#8544 = CARTESIAN_POINT ( 'NONE',  ( -2.000000000000003997, -28.16874999877096997, 5.535898384862238508 ) ) ;
#8545 = ORIENTED_EDGE ( 'NONE', *, *, #15223, .F. ) ;
#8546 = ORIENTED_EDGE ( 'NONE', *, *, #1970, .T. ) ;
#8547 = CARTESIAN_POINT ( 'NONE',  ( 3.756430356250003211, 28.40312499938548640, 8.999999999999992895 ) ) ;
#8548 = ORIENTED_EDGE ( 'NONE', *, *, #8819, .F. ) ;
#8549 = CARTESIAN_POINT ( 'NONE',  ( 3.469446951953614189E-15, 35.50000000000000711, 8.999999999999992895 ) ) ;
#8550 = ORIENTED_EDGE ( 'NONE', *, *, #10784, .F. ) ;
#8551 = B_SPLINE_CURVE_WITH_KNOTS ( 'NONE', 3,
 ( #2997, #530, #6914, #7038, #18819, #6790, #18951, #1036, #18571, #9010, #24837, #12682, #14640, #10696 ),
 .UNSPECIFIED., .F., .F.,
 ( 4, 2, 2, 2, 2, 2, 4 ),
 ( 0.0005975277179059593300, 0.0007548771353729052036, 0.0009122265528398510771, 0.001069575970306796842, 0.001226925387773742824, 0.001541624222707645197, 0.001856323057641547569 ),
 .UNSPECIFIED. ) ;
#8552 = CARTESIAN_POINT ( 'NONE',  ( 18.51293941407127974, 18.51293941407120869, 12.99999999999999112 ) ) ;
#8553 = ORIENTED_EDGE ( 'NONE', *, *, #19593, .T. ) ;
#8554 = CARTESIAN_POINT ( 'NONE',  ( -31.03863125411922752, 1.952785157361987878, 1.000000000000000000 ) ) ;
#8555 = CYLINDRICAL_SURFACE ( 'NONE', #11095, 0.5000000000000004441 ) ;
#8556 = VERTEX_POINT ( 'NONE', #4055 ) ;
#8557 = CARTESIAN_POINT ( 'NONE',  ( -3.756430356249996994, 27.61562499938548143, 8.999999999999992895 ) ) ;
#8558 = CARTESIAN_POINT ( 'NONE',  ( 6.009258394948636914E-15, 29.30312499938549564, 4.662447845253954171 ) ) ;
#8559 = CARTESIAN_POINT ( 'NONE',  ( -3.469446951953614189E-15, -30.00000000000000355, 8.999999999999992895 ) ) ;
#8560 = CARTESIAN_POINT ( 'NONE',  ( 17.67766952966372429, 17.67766952966365324, 12.99999999999999289 ) ) ;
#8561 = CARTESIAN_POINT ( 'NONE',  ( 17.93620544610052647, 17.93620544610046252, 4.662447845253954171 ) ) ;
#8562 = EDGE_CURVE ( 'NONE', #2329, #1175, #21980, .T. ) ;
#8563 = CARTESIAN_POINT ( 'NONE',  ( 3.756430356250004099, 28.77812499938548285, 6.831223922626973533 ) ) ;
#8564 = ADVANCED_FACE ( 'NONE', ( #6149 ), #13883, .F. ) ;
#8565 = CARTESIAN_POINT ( 'NONE',  ( -1.071796769724487230, 26.03259618943233278, 4.999999999999992006 ) ) ;
#8566 = CARTESIAN_POINT ( 'NONE',  ( 20.30280345481878967, 20.30280345481871151, 4.381197846482986158 ) ) ;
#8567 = DIRECTION ( 'NONE',  ( -0.000000000000000000, -0.000000000000000000, 1.000000000000000000 ) ) ;
#8568 = EDGE_CURVE ( 'NONE', #20899, #21834, #17103, .T. ) ;
#8569 = CARTESIAN_POINT ( 'NONE',  ( 5.706339097770929847, 31.50000000000000000, 10.85410196624966517 ) ) ;
#8570 = CARTESIAN_POINT ( 'NONE',  ( 3.756430356249997438, -28.10312499938548569, 11.16877607737301048 ) ) ;
#8571 = ADVANCED_FACE ( 'NONE', ( #3940 ), #16103, .F. ) ;
#8572 = CARTESIAN_POINT ( 'NONE',  ( 3.999999999999972466, -6.690598923241471319, 1.387500000000000844 ) ) ;
#8573 = ORIENTED_EDGE ( 'NONE', *, *, #5167, .T. ) ;
#8574 = CARTESIAN_POINT ( 'NONE',  ( -3.756430356249996994, 25.47812499938548569, 8.999999999999992895 ) ) ;
#8575 = CARTESIAN_POINT ( 'NONE',  ( -4.000000000000003553, -29.08750000000000213, 6.690598923241489970 ) ) ;
#8577 = ORIENTED_EDGE ( 'NONE', *, *, #21163, .F. ) ;
#8576 = CARTESIAN_POINT ( 'NONE',  ( 3.756430356250004099, 27.54062499938548569, 6.831223922626973533 ) ) ;
#8578 = ORIENTED_EDGE ( 'NONE', *, *, #17040, .T. ) ;
#8579 = CARTESIAN_POINT ( 'NONE',  ( 3.756430356250002323, 29.71562499938548640, 11.16877607737301403 ) ) ;
#8580 = LINE ( 'NONE', #6995, #23430 ) ;
#8581 = ORIENTED_EDGE ( 'NONE', *, *, #20182, .F. ) ;
#8582 = VERTEX_POINT ( 'NONE', #9942 ) ;
#8583 = CARTESIAN_POINT ( 'NONE',  ( 3.756430356249996994, -27.27812499938548640, 8.999999999999992895 ) ) ;
#8584 = CARTESIAN_POINT ( 'NONE',  ( -3.756430356249997882, 28.51562499938548711, 8.999999999999992895 ) ) ;
#8585 = DIRECTION ( 'NONE',  ( -1.000000000000000000, -0.000000000000000000, -0.000000000000000000 ) ) ;
#8586 = CARTESIAN_POINT ( 'NONE',  ( -19.82388608118446527, -23.96296185032687376, 1.000000000000000000 ) ) ;
#8587 = AXIS2_PLACEMENT_3D ( 'NONE', #10469, #16765, #2641 ) ;
#8588 = DIRECTION ( 'NONE',  ( 0.000000000000000000, 0.000000000000000000, 1.000000000000000000 ) ) ;
#8589 = CARTESIAN_POINT ( 'NONE',  ( 3.469446951953614189E-15, 40.00000000000000000, 8.999999999999992895 ) ) ;
#8590 = EDGE_CURVE ( 'NONE', #3948, #18495, #14736, .T. ) ;
#8591 = DIRECTION ( 'NONE',  ( -0.000000000000000000, 0.000000000000000000, 1.000000000000000000 ) ) ;
#8592 = CARTESIAN_POINT ( 'NONE',  ( 4.000000000000001776, 25.41250000000000142, 11.30940107675849760 ) ) ;
#8593 = CARTESIAN_POINT ( 'NONE',  ( 20.96136040992792715, 18.30516303196848327, 12.25316411605952283 ) ) ;
#8594 = CARTESIAN_POINT ( 'NONE',  ( 19.62663259444009611, 19.62663259444002151, 4.381197846482986158 ) ) ;
#8595 = DIRECTION ( 'NONE',  ( -0.7289686274214034478, 0.6845471059286972748, 0.000000000000000000 ) ) ;
#8596 = DIRECTION ( 'NONE',  ( 1.000000000000000000, 0.000000000000000000, 0.000000000000000000 ) ) ;
#8597 = CARTESIAN_POINT ( 'NONE',  ( 3.735045420075836212E-15, 26.60312499938547859, 4.662447845253954171 ) ) ;
#8599 = ORIENTED_EDGE ( 'NONE', *, *, #24415, .T. ) ;
#8598 = CYLINDRICAL_SURFACE ( 'NONE', #25825, 0.5000000000000004441 ) ;
#8600 = CARTESIAN_POINT ( 'NONE',  ( 19.15823811790222919, 16.50204073994278531, 5.746835883940462963 ) ) ;
#8601 = CARTESIAN_POINT ( 'NONE',  ( 3.469446951953614189E-15, -8.999999999999992895, 18.00000000000000000 ) ) ;
#8602 = CIRCLE ( 'NONE', #249, 26.00000000000000355 ) ;
#8603 = VERTEX_POINT ( 'NONE', #407 ) ;
#8604 = CARTESIAN_POINT ( 'NONE',  ( 3.469446951953614189E-15, 31.50000000000000000, 8.999999999999992895 ) ) ;
#8605 = CARTESIAN_POINT ( 'NONE',  ( 4.000000000000003553, 27.68124999877096926, 6.690598923241489970 ) ) ;
#8606 = CARTESIAN_POINT ( 'NONE',  ( 1.878215178124998497, -25.89062499938548356, 12.25316411605951927 ) ) ;
#8608 = ORIENTED_EDGE ( 'NONE', *, *, #19673, .T. ) ;
#8607 = CARTESIAN_POINT ( 'NONE',  ( 3.469446951953614189E-15, 25.00000000000000000, 8.999999999999992895 ) ) ;
#8609 = CARTESIAN_POINT ( 'NONE',  ( 4.000000000000003553, -8.999999999999992895, 1.799999999999999600 ) ) ;
#8610 = EDGE_CURVE ( 'NONE', #11941, #8582, #20442, .T. ) ;
#8611 = ORIENTED_EDGE ( 'NONE', *, *, #16875, .T. ) ;
#8612 = CARTESIAN_POINT ( 'NONE',  ( 3.756430356249997882, -26.30312499938548498, 11.16877607737301226 ) ) ;
#8613 = ORIENTED_EDGE ( 'NONE', *, *, #18847, .T. ) ;
#8614 = APPLICATION_CONTEXT ( 'automotive_design' ) ;
#8615 = ORIENTED_EDGE ( 'NONE', *, *, #22350, .T. ) ;
#8616 = CARTESIAN_POINT ( 'NONE',  ( 17.87326343783935911, -25.45105997952923715, 1.000000000000000000 ) ) ;
#8617 = CARTESIAN_POINT ( 'NONE',  ( -1.999999999999995781, 26.89374999877097139, 5.535898384862237620 ) ) ;
#8618 = CARTESIAN_POINT ( 'NONE',  ( 4.000000000000003553, 27.70000000000000284, 8.999999999999992895 ) ) ;
#8619 =( BOUNDED_CURVE ( )  B_SPLINE_CURVE ( 2, ( #9548, #21197, #9307, #25642, #9167, #15198, #11389, #7723, #17292 ),
 .UNSPECIFIED., .F., .F. ) 
 B_SPLINE_CURVE_WITH_KNOTS ( ( 3, 2, 2, 2, 3 ),
 ( 0.9249999999999999334, 0.9333333333333333481, 0.9499999999999999556, 0.9666666666666666741, 0.9749999999999999778 ),
 .UNSPECIFIED. ) 
 CURVE ( )  GEOMETRIC_REPRESENTATION_ITEM ( )  RATIONAL_B_SPLINE_CURVE ( ( 0.9330127018922194093, 0.9330127018922189652, 1.000000000000000000, 0.8660254037844387076, 1.000000000000000000, 0.8660254037844387076, 1.000000000000000000, 0.9330127018922194093, 0.9330127018922194093 ) ) 
 REPRESENTATION_ITEM ( '' )  );
#8620 = CARTESIAN_POINT ( 'NONE',  ( 2.672651547586948120E-15, -13.33755215474602984, 1.940624999385484717 ) ) ;
#8621 =( LENGTH_UNIT ( ) NAMED_UNIT ( * ) SI_UNIT ( .MILLI., .METRE. ) );
#8622 = CARTESIAN_POINT ( 'NONE',  ( -4.000000000000001776, -27.15624999877097423, 11.30940107675849760 ) ) ;
#8623 = CARTESIAN_POINT ( 'NONE',  ( 3.756430356250003655, 26.04062499938548569, 8.999999999999992895 ) ) ;
#8624 = CARTESIAN_POINT ( 'NONE',  ( 18.50088365464961626, 16.98513412679750090, 4.999999999999992006 ) ) ;
#8625 = CARTESIAN_POINT ( 'NONE',  ( -1.859271017917182139E-15, -28.93749999999999645, 12.99999999999999289 ) ) ;
#8626 = CARTESIAN_POINT ( 'NONE',  ( 3.756430356250003655, 28.74062499938548498, 8.999999999999992895 ) ) ;
#8627 = CARTESIAN_POINT ( 'NONE',  ( 0.000000000000000000, 0.000000000000000000, 1.000000000000000000 ) ) ;
#8628 = DIRECTION ( 'NONE',  ( 0.000000000000000000, 0.000000000000000000, 1.000000000000000000 ) ) ;
#8629 = DIRECTION ( 'NONE',  ( 0.000000000000000000, 0.000000000000000000, 1.000000000000000000 ) ) ;
#8630 = CARTESIAN_POINT ( 'NONE',  ( 1.878215178124995832, -27.20312499938548711, 5.746835883940462963 ) ) ;
#8631 = CARTESIAN_POINT ( 'NONE',  ( 1.878215178125000939, 29.67812499938548498, 12.25316411605952283 ) ) ;
#8632 = CARTESIAN_POINT ( 'NONE',  ( -8.831537335106614961E-15, -26.23749999999999716, 12.99999999999999112 ) ) ;
#8633 = DIRECTION ( 'NONE',  ( 1.000000000000000000, 0.000000000000000000, 0.000000000000000000 ) ) ;
#8634 = CARTESIAN_POINT ( 'NONE',  ( 20.92219106202033529, -23.01025686871653875, -2.750000000000000000 ) ) ;
#8635 = EDGE_CURVE ( 'NONE', #4853, #24341, #7209, .T. ) ;
#8636 = VERTEX_POINT ( 'NONE', #10454 ) ;
#8637 = DIRECTION ( 'NONE',  ( 0.000000000000000000, 0.000000000000000000, -1.000000000000000000 ) ) ;
#8639 = ORIENTED_EDGE ( 'NONE', *, *, #25465, .F. ) ;
#8638 = CARTESIAN_POINT ( 'NONE',  ( -7.734255490826573265, 30.12293631110053838, -6.500000000000000000 ) ) ;
#8640 = ORIENTED_EDGE ( 'NONE', *, *, #10574, .F. ) ;
#8641 = ORIENTED_EDGE ( 'NONE', *, *, #2762, .T. ) ;
#8642 = ORIENTED_EDGE ( 'NONE', *, *, #15200, .F. ) ;
#8643 = ORIENTED_EDGE ( 'NONE', *, *, #25329, .T. ) ;
#8644 = DIRECTION ( 'NONE',  ( -0.000000000000000000, -0.000000000000000000, -1.000000000000000000 ) ) ;
#8645 = EDGE_CURVE ( 'NONE', #7861, #19004, #24334, .T. ) ;
#8646 = VERTEX_POINT ( 'NONE', #14402 ) ;
#8647 = LINE ( 'NONE', #6677, #12775 ) ;
#8648 = CARTESIAN_POINT ( 'NONE',  ( 3.756430356250003211, 28.89062499938548356, 6.831223922626973533 ) ) ;
#8649 = CARTESIAN_POINT ( 'NONE',  ( -3.756430356249997882, -11.16877607737301226, 3.665624999385481697 ) ) ;
#8650 = CARTESIAN_POINT ( 'NONE',  ( 21.59775651299582222, 18.94155913503637478, 12.25316411605952283 ) ) ;
#8651 = CARTESIAN_POINT ( 'NONE',  ( -1.499999999999998224, -10.49999999999999289, -6.938893903907228378E-15 ) ) ;
#8652 = CARTESIAN_POINT ( 'NONE',  ( -3.403349963601427053, -25.83240171513484640, 20.00001199999999812 ) ) ;
#8653 = CARTESIAN_POINT ( 'NONE',  ( -3.756430356249996994, -8.999999999999992895, 0.8156249993854814972 ) ) ;
#8654 = CARTESIAN_POINT ( 'NONE',  ( -13.69242354489161251, -27.92360179968368428, 1.000000000000000000 ) ) ;
#8655 = CARTESIAN_POINT ( 'NONE',  ( -3.999999999999996447, -8.999999999999992895, 3.824999999999998401 ) ) ;
#8656 = LINE ( 'NONE', #2265, #25128 ) ;
#8657 = LINE ( 'NONE', #16780, #14273 ) ;
#8658 = CARTESIAN_POINT ( 'NONE',  ( -1.878215178124998497, -12.25316411605951927, 2.803124999385484539 ) ) ;
#8659 = CARTESIAN_POINT ( 'NONE',  ( 3.253724281355068545E-15, 25.50624999877097210, 4.999999999999992006 ) ) ;
#8660 = EDGE_CURVE ( 'NONE', #10164, #4416, #24575, .T. ) ;
#8661 = DIRECTION ( 'NONE',  ( 0.000000000000000000, 0.000000000000000000, 1.000000000000000000 ) ) ;
#8662 = EDGE_LOOP ( 'NONE', ( #23270, #10741, #3293, #23504 ) ) ;
#8663 = ORIENTED_EDGE ( 'NONE', *, *, #9649, .F. ) ;
#8664 = CARTESIAN_POINT ( 'NONE',  ( 0.000000000000000000, 28.74062499938548854, 13.33755215474602984 ) ) ;
#8665 = ADVANCED_FACE ( 'NONE', ( #22362 ), #24720, .T. ) ;
#8666 = ORIENTED_EDGE ( 'NONE', *, *, #25118, .F. ) ;
#8667 = DIRECTION ( 'NONE',  ( -0.000000000000000000, 1.000000000000000000, -0.000000000000000000 ) ) ;
#8668 = VERTEX_POINT ( 'NONE', #14789 ) ;
#8669 = CARTESIAN_POINT ( 'NONE',  ( 5.532151103383234236, 31.50000000000000000, 6.677220593914319657 ) ) ;
#8670 = EDGE_CURVE ( 'NONE', #13117, #822, #8760, .T. ) ;
#8671 = ORIENTED_EDGE ( 'NONE', *, *, #10506, .T. ) ;
#8672 = DIRECTION ( 'NONE',  ( 0.000000000000000000, 0.000000000000000000, 1.000000000000000000 ) ) ;
#8673 = ORIENTED_EDGE ( 'NONE', *, *, #3234, .T. ) ;
#8674 = ADVANCED_FACE ( 'NONE', ( #6414 ), #785, .T. ) ;
#8675 = CARTESIAN_POINT ( 'NONE',  ( -0.4553717634079568755, 38.72245023127407393, 14.76006188199138869 ) ) ;
#8676 = CARTESIAN_POINT ( 'NONE',  ( 3.756430356250003655, 28.74062499938548498, 8.999999999999992895 ) ) ;
#8677 = DIRECTION ( 'NONE',  ( 0.000000000000000000, -1.000000000000000000, 0.000000000000000000 ) ) ;
#8678 = DIRECTION ( 'NONE',  ( 0.000000000000000000, 0.000000000000000000, -1.000000000000000000 ) ) ;
#8679 = FACE_OUTER_BOUND ( 'NONE', #13542, .T. ) ;
#8680 = CARTESIAN_POINT ( 'NONE',  ( -3.999999999999998224, 29.27500000000000568, 8.999999999999992895 ) ) ;
#8681 = CARTESIAN_POINT ( 'NONE',  ( -3.756430356249996994, 28.51562499938548356, 8.999999999999992895 ) ) ;
#8682 = DIRECTION ( 'NONE',  ( 0.000000000000000000, 0.000000000000000000, 1.000000000000000000 ) ) ;
#8683 = CARTESIAN_POINT ( 'NONE',  ( 3.999999999999970690, -11.30940107675851536, 2.212499999999996803 ) ) ;
#8684 = CARTESIAN_POINT ( 'NONE',  ( -14.98253926456298579, 27.25313774936435962, -6.500000000000000000 ) ) ;
#8685 = CARTESIAN_POINT ( 'NONE',  ( 3.469446951953614189E-15, 38.49999999999999289, 8.999999999999992895 ) ) ;
#8686 = CARTESIAN_POINT ( 'NONE',  ( 1.878215178124998497, -27.24062499938548498, 12.25316411605951927 ) ) ;
#8687 = AXIS2_PLACEMENT_3D ( 'NONE', #12327, #16398, #22391 ) ;
#8688 = CARTESIAN_POINT ( 'NONE',  ( 26.49999999999999645, -0.5000000000000000000, 19.00000000000000000 ) ) ;
#8689 = ORIENTED_EDGE ( 'NONE', *, *, #1870, .F. ) ;
#8690 = CARTESIAN_POINT ( 'NONE',  ( 4.000000000000001776, 28.95624999877097494, 11.30940107675849760 ) ) ;
#8691 = CARTESIAN_POINT ( 'NONE',  ( 20.23961848442275269, 18.72386895657063377, 12.99999999999999112 ) ) ;
#8693 = ORIENTED_EDGE ( 'NONE', *, *, #18211, .T. ) ;
#8692 = CARTESIAN_POINT ( 'NONE',  ( 19.94483064597403654, 19.94483064597395838, 4.999999999999992006 ) ) ;
#8694 = VERTEX_POINT ( 'NONE', #4841 ) ;
#8695 = DIRECTION ( 'NONE',  ( -0.000000000000000000, -0.000000000000000000, 1.000000000000000000 ) ) ;
#8696 = LINE ( 'NONE', #22955, #7556 ) ;
#8697 = VECTOR ( 'NONE', #15452, 1000.000000000000000 ) ;
#8698 = VERTEX_POINT ( 'NONE', #22636 ) ;
#8699 = EDGE_CURVE ( 'NONE', #5581, #13483, #22240, .T. ) ;
#8700 = CARTESIAN_POINT ( 'NONE',  ( -2.672651547586948120E-15, -26.49062499938548498, 13.33755215474603162 ) ) ;
#8701 = CARTESIAN_POINT ( 'NONE',  ( 1.859271017917182139E-15, 29.38749999999999929, 12.99999999999999289 ) ) ;
#8702 = CYLINDRICAL_SURFACE ( 'NONE', #25159, 31.10000000000000142 ) ;
#8703 = EDGE_CURVE ( 'NONE', #6938, #23711, #13523, .T. ) ;
#8704 = CARTESIAN_POINT ( 'NONE',  ( 4.000000000000001776, 26.35000000000000497, 8.999999999999992895 ) ) ;
#8705 = CARTESIAN_POINT ( 'NONE',  ( 0.000000000000000000, 25.92812499938548854, 13.33755215474602984 ) ) ;
#8706 = CARTESIAN_POINT ( 'NONE',  ( 21.19421263902459529, 19.67846311117246927, 12.99999999999999467 ) ) ;
#8707 = VECTOR ( 'NONE', #3096, 1000.000000000000000 ) ;
#8708 = SURFACE_SIDE_STYLE ('',( #10540 ) ) ;
#8709 = DIRECTION ( 'NONE',  ( 0.000000000000000000, -0.000000000000000000, 1.000000000000000000 ) ) ;
#8710 = AXIS2_PLACEMENT_3D ( 'NONE', #1595, #5648, #21348 ) ;
#8711 = CARTESIAN_POINT ( 'NONE',  ( 3.959305671612554781E-15, 35.50000000000000711, 12.99999999999999289 ) ) ;
#8712 = CARTESIAN_POINT ( 'NONE',  ( -3.756430356249997438, 25.40312499938548285, 11.16877607737301048 ) ) ;
#8713 = CARTESIAN_POINT ( 'NONE',  ( 3.999999999999996447, -28.31874999877096855, 8.999999999999992895 ) ) ;
#8714 = CARTESIAN_POINT ( 'NONE',  ( 19.92494326818769323, 19.92494326818762218, 13.33755215474602984 ) ) ;
#8715 = CARTESIAN_POINT ( 'NONE',  ( 15.38607408531914089, 20.69846884123782260, 11.16877607737301226 ) ) ;
#8716 = CARTESIAN_POINT ( 'NONE',  ( -24.66042852506104310, -18.28012134629567598, -6.500000000000000000 ) ) ;
#8717 = DIRECTION ( 'NONE',  ( 0.000000000000000000, -0.000000000000000000, 1.000000000000000000 ) ) ;
#8718 = CARTESIAN_POINT ( 'NONE',  ( 2.672651547586948120E-15, 28.62812499938548783, 13.33755215474602984 ) ) ;
#8720 = ORIENTED_EDGE ( 'NONE', *, *, #1575, .T. ) ;
#8719 = DIRECTION ( 'NONE',  ( 1.000000000000000000, 0.000000000000000000, 0.000000000000000000 ) ) ;
#8721 = CARTESIAN_POINT ( 'NONE',  ( -1.071796769724487230, 25.52634618820331269, 4.999999999999992895 ) ) ;
#8722 = CARTESIAN_POINT ( 'NONE',  ( 0.000000000000000000, 10.00000000000000000, 15.00000000000000178 ) ) ;
#8723 = ORIENTED_EDGE ( 'NONE', *, *, #18735, .F. ) ;
#8724 = CARTESIAN_POINT ( 'NONE',  ( -11.44867358849371541, -28.91604871112453168, 1.000000000000000000 ) ) ;
#8725 = CARTESIAN_POINT ( 'NONE',  ( 3.752267015613588906E-15, 27.30624999877097281, 4.381197846482986158 ) ) ;
#8726 = CARTESIAN_POINT ( 'NONE',  ( -1.878215178125004048, -26.11562499938548498, 5.746835883940462963 ) ) ;
#8728 = VERTEX_POINT ( 'NONE', #3249 ) ;
#8727 = DIRECTION ( 'NONE',  ( 1.000000000000000000, 0.000000000000000000, 0.000000000000000000 ) ) ;
#8729 = CARTESIAN_POINT ( 'NONE',  ( 26.52310962334739486, -16.23990935651726275, -2.750000000000000000 ) ) ;
#8730 = VECTOR ( 'NONE', #16227, 1000.000000000000000 ) ;
#8731 = ORIENTED_EDGE ( 'NONE', *, *, #5020, .F. ) ;
#8732 = EDGE_CURVE ( 'NONE', #22681, #10320, #7632, .T. ) ;
#8733 = CARTESIAN_POINT ( 'NONE',  ( -1.878215178125000939, -25.51562499938548356, 12.25316411605952283 ) ) ;
#8734 = VERTEX_POINT ( 'NONE', #7054 ) ;
#8735 = CIRCLE ( 'NONE', #5331, 31.10000000000000142 ) ;
#8736 = ORIENTED_EDGE ( 'NONE', *, *, #21132, .F. ) ;
#8737 = SURFACE_SIDE_STYLE ('',( #4428 ) ) ;
#8738 = CARTESIAN_POINT ( 'NONE',  ( -2.003086131649545506E-15, 26.04062499938549280, 13.33755215474602984 ) ) ;
#8740 = EDGE_CURVE ( 'NONE', #24433, #10494, #9022, .T. ) ;
#8739 = CIRCLE ( 'NONE', #806, 2.000000000000000000 ) ;
#8741 = CARTESIAN_POINT ( 'NONE',  ( 0.000000000000000000, 0.000000000000000000, -6.500000000000000000 ) ) ;
#8742 = CARTESIAN_POINT ( 'NONE',  ( -3.756430356249997882, -11.16877607737301226, 2.765624999385486227 ) ) ;
#8743 = DIRECTION ( 'NONE',  ( 0.000000000000000000, -0.000000000000000000, 1.000000000000000000 ) ) ;
#8744 = PRESENTATION_LAYER_ASSIGNMENT (  '', '', ( #20016 ) ) ;
#8745 = CARTESIAN_POINT ( 'NONE',  ( 3.756430356250004099, 27.87812499938548427, 6.831223922626973533 ) ) ;
#8746 = EDGE_CURVE ( 'NONE', #18387, #19344, #24852, .T. ) ;
#8747 = CARTESIAN_POINT ( 'NONE',  ( -31.03863125411927371, -1.952785157361310198, 1.000000000000000000 ) ) ;
#8748 = VECTOR ( 'NONE', #15045, 1000.000000000000000 ) ;
#8749 = CARTESIAN_POINT ( 'NONE',  ( 10.08469938919499320, 29.41953157733090762, -6.500000000000000000 ) ) ;
#8750 = CARTESIAN_POINT ( 'NONE',  ( 3.756430356250003655, 29.64062499938548356, 8.999999999999992895 ) ) ;
#8751 = CARTESIAN_POINT ( 'NONE',  ( 18.88296798233768214, 20.39871751018965895, 4.999999999999992006 ) ) ;
#8752 = CARTESIAN_POINT ( 'NONE',  ( -13.69242354489114177, 27.92360179968391165, -6.500000000000000000 ) ) ;
#8753 = CARTESIAN_POINT ( 'NONE',  ( 2.000000000000000888, -12.46410161513774817, 0.7687499987709678351 ) ) ;
#8754 = CARTESIAN_POINT ( 'NONE',  ( 3.756430356249997882, -26.41562499938548569, 11.16877607737301226 ) ) ;
#8755 = DIRECTION ( 'NONE',  ( 0.000000000000000000, -0.000000000000000000, 1.000000000000000000 ) ) ;
#8756 = AXIS2_PLACEMENT_3D ( 'NONE', #25401, #3304, #19642 ) ;
#8757 = CYLINDRICAL_SURFACE ( 'NONE', #9547, 4.000000000000000000 ) ;
#8759 = CARTESIAN_POINT ( 'NONE',  ( -3.397863563849436108, 30.85476721088031482, 1.000000000000000000 ) ) ;
#8758 = CIRCLE ( 'NONE', #1669, 31.10000000000000142 ) ;
#8760 = LINE ( 'NONE', #18451, #6793 ) ;
#8761 = ORIENTED_EDGE ( 'NONE', *, *, #2952, .F. ) ;
#8762 = DIRECTION ( 'NONE',  ( 1.000000000000000000, 0.000000000000000000, 0.000000000000000000 ) ) ;
#8764 = ORIENTED_EDGE ( 'NONE', *, *, #144, .F. ) ;
#8763 = CARTESIAN_POINT ( 'NONE',  ( -28.72825533807142051, -11.91206721063020701, -2.750000000000000000 ) ) ;
#8765 =( BOUNDED_CURVE ( )  B_SPLINE_CURVE ( 2, ( #10952, #20501, #12032, #4817, #22464, #24825, #23954, #1025, #4690 ),
 .UNSPECIFIED., .F., .F. ) 
 B_SPLINE_CURVE_WITH_KNOTS ( ( 3, 2, 2, 2, 3 ),
 ( 0.2250000000000000056, 0.2333333333333333370, 0.2500000000000000000, 0.2666666666666666630, 0.2750000000000000222 ),
 .UNSPECIFIED. ) 
 CURVE ( )  GEOMETRIC_REPRESENTATION_ITEM ( )  RATIONAL_B_SPLINE_CURVE ( ( 0.9330127018922194093, 0.9330127018922194093, 1.000000000000000000, 0.8660254037844387076, 1.000000000000000000, 0.8660254037844387076, 1.000000000000000000, 0.9330127018922191873, 0.9330127018922194093 ) ) 
 REPRESENTATION_ITEM ( '' )  );
#8766 = VERTEX_POINT ( 'NONE', #14913 ) ;
#8767 = VECTOR ( 'NONE', #19376, 1000.000000000000000 ) ;
#8768 = VERTEX_POINT ( 'NONE', #11225 ) ;
#8769 = ORIENTED_EDGE ( 'NONE', *, *, #20034, .F. ) ;
#8770 = ORIENTED_EDGE ( 'NONE', *, *, #5089, .F. ) ;
#8771 = ADVANCED_FACE ( 'NONE', ( #15042 ), #17135, .F. ) ;
#8772 = DIRECTION ( 'NONE',  ( 0.000000000000000000, 0.000000000000000000, -1.000000000000000000 ) ) ;
#8773 =( BOUNDED_CURVE ( )  B_SPLINE_CURVE ( 2, ( #7310, #25475, #15549, #5469, #1427, #9780, #17760, #11738, #23385 ),
 .UNSPECIFIED., .F., .F. ) 
 B_SPLINE_CURVE_WITH_KNOTS ( ( 3, 2, 2, 2, 3 ),
 ( 0.3250000000000000111, 0.3333333333333333148, 0.3499999999999999778, 0.3666666666666666408, 0.3750000000000000000 ),
 .UNSPECIFIED. ) 
 CURVE ( )  GEOMETRIC_REPRESENTATION_ITEM ( )  RATIONAL_B_SPLINE_CURVE ( ( 0.9330127018922194093, 0.9330127018922196314, 1.000000000000000000, 0.8660254037844387076, 1.000000000000000000, 0.8660254037844387076, 1.000000000000000000, 0.9330127018922194093, 0.9330127018922194093 ) ) 
 REPRESENTATION_ITEM ( '' )  );
#8774 = CIRCLE ( 'NONE', #2515, 31.10000000000000142 ) ;
#8775 = ORIENTED_EDGE ( 'NONE', *, *, #22800, .T. ) ;
#8776 = CARTESIAN_POINT ( 'NONE',  ( -29.07785765677917311, 9.610428525061202265, -6.500000000000000000 ) ) ;
#8777 = CARTESIAN_POINT ( 'NONE',  ( -3.756430356249996994, 27.72812499938548569, 8.999999999999992895 ) ) ;
#8778 = VECTOR ( 'NONE', #9960, 1000.000000000000000 ) ;
#8779 = EDGE_CURVE ( 'NONE', #18169, #5530, #3387, .T. ) ;
#8780 = CARTESIAN_POINT ( 'NONE',  ( 3.756430356250004099, -6.831223922626973533, 3.890624999385483562 ) ) ;
#8781 = FACE_OUTER_BOUND ( 'NONE', #4977, .T. ) ;
#8782 = CARTESIAN_POINT ( 'NONE',  ( 19.52492222951535439, 22.18111960747465261, 12.25316411605951927 ) ) ;
#8783 = DIRECTION ( 'NONE',  ( 0.000000000000000000, 0.000000000000000000, -1.000000000000000000 ) ) ;
#8784 = EDGE_CURVE ( 'NONE', #21413, #23824, #22883, .T. ) ;
#8785 = CARTESIAN_POINT ( 'NONE',  ( -2.899999999999996358, -8.999999999999992895, -10.00000000000000000 ) ) ;
#8786 = VECTOR ( 'NONE', #19210, 1000.000000000000000 ) ;
#8787 = CARTESIAN_POINT ( 'NONE',  ( -3.756430356249997882, -11.16877607737301226, 3.103124999385483029 ) ) ;
#8788 = DIRECTION ( 'NONE',  ( -0.8660254037844397068, 0.4999999999999983347, 0.000000000000000000 ) ) ;
#8789 = DIRECTION ( 'NONE',  ( 0.000000000000000000, 0.000000000000000000, -1.000000000000000000 ) ) ;
#8790 = LINE ( 'NONE', #24482, #18447 ) ;
#8791 = CARTESIAN_POINT ( 'NONE',  ( -14.98253926456356666, -27.25313774936403988, -6.500000000000000000 ) ) ;
#8792 = CARTESIAN_POINT ( 'NONE',  ( 1.878215178125000939, -12.25316411605952283, 1.978124999385485250 ) ) ;
#8793 = CIRCLE ( 'NONE', #23409, 0.4999999999999998890 ) ;
#8794 = CARTESIAN_POINT ( 'NONE',  ( 27.92360179968377309, 13.69242354489143665, 1.000000000000000000 ) ) ;
#8795 = DIRECTION ( 'NONE',  ( 0.7289686274214101092, -0.6845471059286901694, 0.000000000000000000 ) ) ;
#8796 = VERTEX_POINT ( 'NONE', #23263 ) ;
#8797 = ORIENTED_EDGE ( 'NONE', *, *, #12468, .F. ) ;
#8798 = CARTESIAN_POINT ( 'NONE',  ( 1.878215178125001605, 28.77812499938549351, 12.25316411605952283 ) ) ;
#8799 = AXIS2_PLACEMENT_3D ( 'NONE', #10218, #18216, #14300 ) ;
#8800 = ORIENTED_EDGE ( 'NONE', *, *, #12347, .T. ) ;
#8801 = DIRECTION ( 'NONE',  ( 0.000000000000000000, 0.000000000000000000, -1.000000000000000000 ) ) ;
#8802 = ORIENTED_EDGE ( 'NONE', *, *, #4870, .F. ) ;
#8803 = CARTESIAN_POINT ( 'NONE',  ( 3.756430356249996994, -26.37812499938548783, 8.999999999999992895 ) ) ;
#8804 = ORIENTED_EDGE ( 'NONE', *, *, #17695, .F. ) ;
#8805 = CARTESIAN_POINT ( 'NONE',  ( -1.999999999999994893, 27.79374999877096997, 5.535898384862237620 ) ) ;
#8806 = AXIS2_PLACEMENT_3D ( 'NONE', #6064, #12067, #16017 ) ;
#8807 = ORIENTED_EDGE ( 'NONE', *, *, #11521, .F. ) ;
#8808 = DIRECTION ( 'NONE',  ( 0.000000000000000000, 0.000000000000000000, 1.000000000000000000 ) ) ;
#8809 = CARTESIAN_POINT ( 'NONE',  ( -3.999999999999996003, 25.63749999999999929, 6.690598923241487306 ) ) ;
#8810 = DIRECTION ( 'NONE',  ( -0.9048270524660170233, 0.4257792915650782661, 0.000000000000000000 ) ) ;
#8811 = AXIS2_PLACEMENT_3D ( 'NONE', #20488, #2584, #18547 ) ;
#8812 = CIRCLE ( 'NONE', #16346, 31.10000000000000142 ) ;
#8813 = EDGE_CURVE ( 'NONE', #1657, #22706, #19774, .T. ) ;
#8814 = CARTESIAN_POINT ( 'NONE',  ( -3.999999999999996447, -8.999999999999992895, 18.00000000000000000 ) ) ;
#8815 = CARTESIAN_POINT ( 'NONE',  ( 3.959305671612554781E-15, 35.50000000000000711, 12.99999999999999289 ) ) ;
#8816 = CARTESIAN_POINT ( 'NONE',  ( 19.55598568231966539, 16.89978830436022150, 5.746835883940462963 ) ) ;
#8817 = VECTOR ( 'NONE', #8190, 1000.000000000000000 ) ;
#8818 = CIRCLE ( 'NONE', #24249, 31.10000000000000142 ) ;
#8819 = EDGE_CURVE ( 'NONE', #24829, #21754, #8907, .T. ) ;
#8820 = CARTESIAN_POINT ( 'NONE',  ( -3.756430356249997882, 27.65312499938548640, 11.16877607737301226 ) ) ;
#8821 = CARTESIAN_POINT ( 'NONE',  ( -3.999999999999995559, 26.08749999999999503, 6.690598923241487306 ) ) ;
#8822 = CARTESIAN_POINT ( 'NONE',  ( 2.451530025008918923, -31.00322564728515928, -6.500000000000000000 ) ) ;
#8823 = AXIS2_PLACEMENT_3D ( 'NONE', #25695, #7777, #18124 ) ;
#8824 = ORIENTED_EDGE ( 'NONE', *, *, #10435, .T. ) ;
#8825 = CARTESIAN_POINT ( 'NONE',  ( -2.000000000000003997, -25.07499999999999929, 5.535898384862238508 ) ) ;
#8826 = EDGE_CURVE ( 'NONE', #19703, #3427, #22438, .T. ) ;
#8827 = CARTESIAN_POINT ( 'NONE',  ( -3.999999999999996447, 26.51874999877097494, 8.999999999999992895 ) ) ;
#8828 = AXIS2_PLACEMENT_3D ( 'NONE', #6629, #22855, #10806 ) ;
#8829 = CARTESIAN_POINT ( 'NONE',  ( 3.756430356249996105, -28.02812499938548996, 6.831223922626973533 ) ) ;
#8830 = VECTOR ( 'NONE', #1074, 1000.000000000000000 ) ;
#8831 = CYLINDRICAL_SURFACE ( 'NONE', #15856, 0.5000000000000004441 ) ;
#8832 = CARTESIAN_POINT ( 'NONE',  ( 4.000000000000003553, 29.89374999877096784, 8.999999999999992895 ) ) ;
#8833 = DIRECTION ( 'NONE',  ( 0.8443279255020205154, 0.5358267949789882190, 0.000000000000000000 ) ) ;
#8835 = VERTEX_POINT ( 'NONE', #20929 ) ;
#8834 = DIRECTION ( 'NONE',  ( -1.000000000000000000, 0.000000000000000000, 0.000000000000000000 ) ) ;
#8836 = EDGE_LOOP ( 'NONE', ( #3812, #10006, #16946, #5070 ) ) ;
#8837 = LINE ( 'NONE', #20330, #10372 ) ;
#8838 = AXIS2_PLACEMENT_3D ( 'NONE', #2166, #21905, #16034 ) ;
#8839 = CYLINDRICAL_SURFACE ( 'NONE', #9225, 0.5000000000000000000 ) ;
#8840 = ORIENTED_EDGE ( 'NONE', *, *, #23445, .F. ) ;
#8841 = EDGE_CURVE ( 'NONE', #14526, #10206, #3012, .T. ) ;
#8842 = CARTESIAN_POINT ( 'NONE',  ( 3.756430356249996105, -27.24062499938548498, 6.831223922626973533 ) ) ;
#8843 = CARTESIAN_POINT ( 'NONE',  ( 1.500000000000001776, -10.49999999999999289, 30.00000000000000355 ) ) ;
#8844 = CARTESIAN_POINT ( 'NONE',  ( -3.756430356249996549, 26.71562499938548996, 8.999999999999992895 ) ) ;
#8845 = AXIS2_PLACEMENT_3D ( 'NONE', #6576, #8672, #22680 ) ;
#8846 = CARTESIAN_POINT ( 'NONE',  ( 7.901901826148023498E-15, 26.23750000000000426, 12.99999999999999112 ) ) ;
#8847 = CARTESIAN_POINT ( 'NONE',  ( 4.000000000000005329, 25.41250000000000497, 11.30940107675849760 ) ) ;
#8848 = VECTOR ( 'NONE', #4707, 1000.000000000000000 ) ;
#8849 = AXIS2_PLACEMENT_3D ( 'NONE', #9164, #13224, #8783 ) ;
#8850 = CARTESIAN_POINT ( 'NONE',  ( 3.756430356250003655, -8.999999999999992895, 4.190624999385480720 ) ) ;
#8851 = DIRECTION ( 'NONE',  ( 1.000000000000000000, 0.000000000000000000, 0.000000000000000000 ) ) ;
#8852 = DIRECTION ( 'NONE',  ( 1.000000000000000000, 0.000000000000000000, 0.000000000000000000 ) ) ;
#8853 = EDGE_CURVE ( 'NONE', #7580, #25532, #11493, .T. ) ;
#8854 = DIRECTION ( 'NONE',  ( 1.000000000000000000, 0.000000000000000000, -0.000000000000000000 ) ) ;
#8855 = CIRCLE ( 'NONE', #3017, 31.10000000000000142 ) ;
#8856 = LINE ( 'NONE', #4402, #5902 ) ;
#8857 = CARTESIAN_POINT ( 'NONE',  ( 16.55955693104344206, 22.21641118053575426, 8.999999999999992895 ) ) ;
#8858 = CARTESIAN_POINT ( 'NONE',  ( 5.577813053751546416E-15, 25.33750000000000213, 12.99999999999999289 ) ) ;
#8859 = CARTESIAN_POINT ( 'NONE',  ( 17.91631806831418317, 17.91631806831411922, 13.61880215351699874 ) ) ;
#8860 = CARTESIAN_POINT ( 'NONE',  ( 19.44991966514168169, 16.79372228718224491, 12.25316411605952283 ) ) ;
#8861 = EDGE_CURVE ( 'NONE', #19775, #1445, #23930, .T. ) ;
#8862 = CARTESIAN_POINT ( 'NONE',  ( 1.071796769724498999, 27.60759618943233207, 12.99999999999998757 ) ) ;
#8863 = CARTESIAN_POINT ( 'NONE',  ( -3.897863563850083146, -30.85476721088024021, -6.500000000000000000 ) ) ;
#8864 = CARTESIAN_POINT ( 'NONE',  ( 1.878215178125000939, 27.76562499938548356, 12.25316411605952283 ) ) ;
#8865 = EDGE_CURVE ( 'NONE', #17200, #10488, #8068, .T. ) ;
#8866 = CYLINDRICAL_SURFACE ( 'NONE', #23340, 31.10000000000000142 ) ;
#8867 = AXIS2_PLACEMENT_3D ( 'NONE', #23406, #11376, #24981 ) ;
#8868 = CARTESIAN_POINT ( 'NONE',  ( -1.071796769724487453, 25.71115380933864003, 12.99999999999999467 ) ) ;
#8869 = CARTESIAN_POINT ( 'NONE',  ( 22.72022476213122744, 17.06337051263877669, 6.690598923241489970 ) ) ;
#8870 = EDGE_LOOP ( 'NONE', ( #10083, #3353, #21650, #21089 ) ) ;
#8871 = CARTESIAN_POINT ( 'NONE',  ( -3.999999999999997335, 28.86250000000000071, 11.30940107675849404 ) ) ;
#8872 = CARTESIAN_POINT ( 'NONE',  ( 3.752267015613588906E-15, 29.10624999877096997, 4.381197846482986158 ) ) ;
#8873 = CARTESIAN_POINT ( 'NONE',  ( -1.878215178125004048, -27.91562499938548569, 5.746835883940462963 ) ) ;
#8875 = ORIENTED_EDGE ( 'NONE', *, *, #5808, .F. ) ;
#8874 = CARTESIAN_POINT ( 'NONE',  ( 30.24338421796780807, 7.248980000274215740, 1.000000000000000000 ) ) ;
#8876 = AXIS2_PLACEMENT_3D ( 'NONE', #24284, #15928, #20219 ) ;
#8877 = LINE ( 'NONE', #16860, #24174 ) ;
#8878 = VERTEX_POINT ( 'NONE', #11878 ) ;
#8879 = CARTESIAN_POINT ( 'NONE',  ( 1.878215178124995832, -26.19062499938548427, 5.746835883940462963 ) ) ;
#8880 = ORIENTED_EDGE ( 'NONE', *, *, #4692, .T. ) ;
#8881 = ORIENTED_EDGE ( 'NONE', *, *, #21260, .F. ) ;
#8882 = CYLINDRICAL_SURFACE ( 'NONE', #16417, 0.5000000000000004441 ) ;
#8884 = CARTESIAN_POINT ( 'NONE',  ( 3.756430356250003211, 28.40312499938548640, 8.999999999999992895 ) ) ;
#8883 = CIRCLE ( 'NONE', #14720, 4.000000000000000000 ) ;
#8885 = DIRECTION ( 'NONE',  ( 1.000000000000000000, 0.000000000000000000, 0.000000000000000000 ) ) ;
#8886 = AXIS2_PLACEMENT_3D ( 'NONE', #5740, #25633, #14250 ) ;
#8887 = CARTESIAN_POINT ( 'NONE',  ( -1.878215178124995832, -5.746835883940462963, 0.8531249993854843616 ) ) ;
#8888 =( NAMED_UNIT ( * ) SI_UNIT ( $, .STERADIAN. ) SOLID_ANGLE_UNIT ( ) );
#8889 = DIRECTION ( 'NONE',  ( 0.000000000000000000, 0.000000000000000000, -1.000000000000000000 ) ) ;
#8890 = CARTESIAN_POINT ( 'NONE',  ( 3.735045420075836212E-15, 27.50312499938548783, 4.662447845253954171 ) ) ;
#8891 = AXIS2_PLACEMENT_3D ( 'NONE', #15838, #14135, #5643 ) ;
#8892 = CARTESIAN_POINT ( 'NONE',  ( 21.23398739633539023, 19.71823786848327131, 12.99999999999999467 ) ) ;
#8893 = CARTESIAN_POINT ( 'NONE',  ( -23.64116323484252291, -20.20656826142258211, -6.500000000000000000 ) ) ;
#8894 = UNCERTAINTY_MEASURE_WITH_UNIT (LENGTH_MEASURE( 1.000000000000000082E-05 ), #1543, 'distance_accuracy_value', 'NONE');
#8895 = UNCERTAINTY_MEASURE_WITH_UNIT (LENGTH_MEASURE( 1.000000000000000082E-05 ), #19711, 'distance_accuracy_value', 'NONE');
#8896 = CARTESIAN_POINT ( 'NONE',  ( -3.756430356249996994, 28.96562499938548285, 8.999999999999992895 ) ) ;
#8897 = DIRECTION ( 'NONE',  ( -0.7705132427757935831, -0.6374239897486843054, 0.000000000000000000 ) ) ;
#8898 = CARTESIAN_POINT ( 'NONE',  ( -29.99470236596038220, -8.217531866530892515, -6.500000000000000000 ) ) ;
#8899 = CARTESIAN_POINT ( 'NONE',  ( 2.620986760973688460E-15, -13.61880215351699874, 0.7312499987709675242 ) ) ;
#8900 = EDGE_CURVE ( 'NONE', #13187, #4613, #17258, .T. ) ;
#8901 = CARTESIAN_POINT ( 'NONE',  ( -3.756430356250003655, -27.05312499938548498, 8.999999999999992895 ) ) ;
#8902 = LINE ( 'NONE', #13203, #7747 ) ;
#8903 = ADVANCED_FACE ( 'NONE', ( #3909, #19967 ), #19730, .F. ) ;
#8904 = CYLINDRICAL_SURFACE ( 'NONE', #20385, 0.5000000000000004441 ) ;
#8905 = AXIS2_PLACEMENT_3D ( 'NONE', #7589, #11380, #7452 ) ;
#8906 = CARTESIAN_POINT ( 'NONE',  ( 0.000000000000000000, 0.000000000000000000, 1.000000000000000000 ) ) ;
#8907 = LINE ( 'NONE', #25105, #1387 ) ;
#8908 = ORIENTED_EDGE ( 'NONE', *, *, #8732, .T. ) ;
#8909 = DIRECTION ( 'NONE',  ( 0.000000000000000000, 1.000000000000000000, 0.000000000000000000 ) ) ;
#8911 = EDGE_LOOP ( 'NONE', ( #22109, #646, #15839, #17067 ) ) ;
#8910 = CARTESIAN_POINT ( 'NONE',  ( -11.91206721063072216, -28.72825533807120735, -2.750000000000000000 ) ) ;
#8912 = EDGE_CURVE ( 'NONE', #421, #22340, #25121, .T. ) ;
#8913 = CIRCLE ( 'NONE', #21017, 0.5000000000000007772 ) ;
#8914 = ORIENTED_EDGE ( 'NONE', *, *, #11059, .T. ) ;
#8915 = ORIENTED_EDGE ( 'NONE', *, *, #12866, .F. ) ;
#8916 = ORIENTED_EDGE ( 'NONE', *, *, #10895, .T. ) ;
#8917 = EDGE_LOOP ( 'NONE', ( #23023, #3577, #703, #12627 ) ) ;
#8918 = CARTESIAN_POINT ( 'NONE',  ( -24.27856662945513477, -19.43607991388973488, 1.000000000000000000 ) ) ;
#8919 = ORIENTED_EDGE ( 'NONE', *, *, #17773, .F. ) ;
#8920 = CARTESIAN_POINT ( 'NONE',  ( 4.000000000000003553, -8.999999999999992895, 18.00000000000000000 ) ) ;
#8921 = CARTESIAN_POINT ( 'NONE',  ( -1.878215178124998497, 29.60312499938548569, 12.25316411605951927 ) ) ;
#8922 = STYLED_ITEM ( 'NONE', ( #2468 ), #22510 ) ;
#8923 = CARTESIAN_POINT ( 'NONE',  ( -3.756430356249997882, -11.16877607737301226, 0.4031249993854806868 ) ) ;
#8924 = CYLINDRICAL_SURFACE ( 'NONE', #10018, 4.000000000000000000 ) ;
#8925 = CARTESIAN_POINT ( 'NONE',  ( -4.000000000000003553, -25.39374999877096784, 8.999999999999992895 ) ) ;
#8926 = CARTESIAN_POINT ( 'NONE',  ( -3.756430356249995661, 26.79062499938548925, 6.831223922626973533 ) ) ;
#8927 = VECTOR ( 'NONE', #4823, 1000.000000000000000 ) ;
#8928 = DIRECTION ( 'NONE',  ( 1.000000000000000000, 0.000000000000000000, 0.000000000000000000 ) ) ;
#8929 = CARTESIAN_POINT ( 'NONE',  ( 4.000000000000003553, -8.999999999999992895, 0.000000000000000000 ) ) ;
#8930 = CARTESIAN_POINT ( 'NONE',  ( 3.897863563849651936, -30.85476721088028640, -6.500000000000000000 ) ) ;
#8931 = DIRECTION ( 'NONE',  ( 0.000000000000000000, -1.000000000000000000, 0.000000000000000000 ) ) ;
#8932 = CARTESIAN_POINT ( 'NONE',  ( -5.796869523101029209, 38.54567717719766762, 7.639754566698839788 ) ) ;
#8933 = EDGE_CURVE ( 'NONE', #13400, #4609, #14445, .T. ) ;
#8934 =( BOUNDED_CURVE ( )  B_SPLINE_CURVE ( 2, ( #18154, #13831, #17753, #12115, #4138, #22051, #19830, #7685, #14220 ),
 .UNSPECIFIED., .F., .F. ) 
 B_SPLINE_CURVE_WITH_KNOTS ( ( 3, 2, 2, 2, 3 ),
 ( 0.4250000000000000444, 0.4333333333333333481, 0.4500000000000000111, 0.4666666666666666741, 0.4750000000000000333 ),
 .UNSPECIFIED. ) 
 CURVE ( )  GEOMETRIC_REPRESENTATION_ITEM ( )  RATIONAL_B_SPLINE_CURVE ( ( 0.9330127018922194093, 0.9330127018922196314, 1.000000000000000000, 0.8660254037844387076, 1.000000000000000000, 0.8660254037844387076, 1.000000000000000000, 0.9330127018922191873, 0.9330127018922194093 ) ) 
 REPRESENTATION_ITEM ( '' )  );
#8935 = LINE ( 'NONE', #20816, #17185 ) ;
#8936 = DIRECTION ( 'NONE',  ( 0.000000000000000000, 0.000000000000000000, -1.000000000000000000 ) ) ;
#8937 = EDGE_CURVE ( 'NONE', #14948, #15879, #18102, .T. ) ;
#8938 = CARTESIAN_POINT ( 'NONE',  ( 3.999999999999995559, -26.53750000000000142, 6.690598923241487306 ) ) ;
#8939 = CARTESIAN_POINT ( 'NONE',  ( -1.952785157361201618, 31.03863125411927371, -6.500000000000000000 ) ) ;
#8940 = ORIENTED_EDGE ( 'NONE', *, *, #24313, .F. ) ;
#8941 = ORIENTED_EDGE ( 'NONE', *, *, #5630, .F. ) ;
#8942 =( BOUNDED_CURVE ( )  B_SPLINE_CURVE ( 2, ( #1948, #16076, #3911, #14376, #18170, #17895, #19969, #2074, #16468 ),
 .UNSPECIFIED., .F., .F. ) 
 B_SPLINE_CURVE_WITH_KNOTS ( ( 3, 2, 2, 2, 3 ),
 ( 0.3750000000000000000, 0.3833333333333333592, 0.4000000000000000222, 0.4166666666666666852, 0.4250000000000000444 ),
 .UNSPECIFIED. ) 
 CURVE ( )  GEOMETRIC_REPRESENTATION_ITEM ( )  RATIONAL_B_SPLINE_CURVE ( ( 0.9330127018922194093, 0.9330127018922194093, 1.000000000000000000, 0.8660254037844387076, 1.000000000000000000, 0.8660254037844387076, 1.000000000000000000, 0.9330127018922191873, 0.9330127018922194093 ) ) 
 REPRESENTATION_ITEM ( '' )  );
#8943 = VERTEX_POINT ( 'NONE', #11751 ) ;
#8944 = DIRECTION ( 'NONE',  ( 0.000000000000000000, 0.000000000000000000, 1.000000000000000000 ) ) ;
#8945 =( GEOMETRIC_REPRESENTATION_CONTEXT ( 3 ) GLOBAL_UNCERTAINTY_ASSIGNED_CONTEXT ( ( #4954 ) ) GLOBAL_UNIT_ASSIGNED_CONTEXT ( ( #6137, #12406, #2093 ) ) REPRESENTATION_CONTEXT ( 'NONE', 'WORKASPACE' ) );
#8946 = ORIENTED_EDGE ( 'NONE', *, *, #25469, .F. ) ;
#8947 = CARTESIAN_POINT ( 'NONE',  ( -3.756430356250002323, -26.11562499938548498, 11.16877607737301226 ) ) ;
#8948 = ORIENTED_EDGE ( 'NONE', *, *, #12027, .T. ) ;
#8949 = EDGE_CURVE ( 'NONE', #13787, #4937, #19331, .T. ) ;
#8950 = VECTOR ( 'NONE', #7388, 1000.000000000000000 ) ;
#8951 = ORIENTED_EDGE ( 'NONE', *, *, #15959, .T. ) ;
#8952 = CARTESIAN_POINT ( 'NONE',  ( 1.057460391440397258E-14, -29.16249999999999787, 4.999999999999992006 ) ) ;
#8953 = CARTESIAN_POINT ( 'NONE',  ( -3.756430356249995661, 28.47812499938548569, 6.831223922626973533 ) ) ;
#8954 = CARTESIAN_POINT ( 'NONE',  ( 19.18911027444997686, 19.18911027444989870, 12.99999999999999112 ) ) ;
#8955 = DIRECTION ( 'NONE',  ( 0.000000000000000000, 0.000000000000000000, 1.000000000000000000 ) ) ;
#8956 = CARTESIAN_POINT ( 'NONE',  ( 21.65113613650334301, 22.32573188046921331, 1.000000000000000000 ) ) ;
#8957 = CARTESIAN_POINT ( 'NONE',  ( 20.19238178538755690, 17.53618440742811302, 5.746835883940462963 ) ) ;
#8958 = CARTESIAN_POINT ( 'NONE',  ( 3.834746474454188013E-15, 28.26249999999999929, 4.999999999999992006 ) ) ;
#8959 = CARTESIAN_POINT ( 'NONE',  ( -3.999999999999996447, 26.12500000000000355, 8.999999999999992895 ) ) ;
#8960 = CARTESIAN_POINT ( 'NONE',  ( 16.31415173562648491, 21.62654649154516306, 8.999999999999992895 ) ) ;
#8961 = DIRECTION ( 'NONE',  ( 1.000000000000000000, 0.000000000000000000, 0.000000000000000000 ) ) ;
#8962 = ORIENTED_EDGE ( 'NONE', *, *, #8461, .T. ) ;
#8963 = CARTESIAN_POINT ( 'NONE',  ( 8.012344526598182026E-15, 28.65624999877097778, 4.381197846482986158 ) ) ;
#8964 = CARTESIAN_POINT ( 'NONE',  ( 1.878215178124995832, -27.09062499938548640, 5.746835883940462963 ) ) ;
#8965 = LINE ( 'NONE', #25297, #8323 ) ;
#8966 = EDGE_CURVE ( 'NONE', #3531, #56, #11404, .T. ) ;
#8967 = CARTESIAN_POINT ( 'NONE',  ( 2.000000000000003997, 29.06874999877096855, 5.535898384862238508 ) ) ;
#8968 = DIRECTION ( 'NONE',  ( 1.000000000000000000, 0.000000000000000000, -0.000000000000000000 ) ) ;
#8970 = ORIENTED_EDGE ( 'NONE', *, *, #25631, .F. ) ;
#8969 = CARTESIAN_POINT ( 'NONE',  ( 3.756430356250003211, 29.30312499938548498, 8.999999999999992895 ) ) ;
#8971 = ORIENTED_EDGE ( 'NONE', *, *, #12288, .F. ) ;
#8972 = DIRECTION ( 'NONE',  ( 0.6374239897486995154, 0.7705132427757811486, 0.000000000000000000 ) ) ;
#8973 = PRODUCT_DEFINITION_FORMATION_WITH_SPECIFIED_SOURCE ( 'ANY', '', #18425, .NOT_KNOWN. ) ;
#8974 = CARTESIAN_POINT ( 'NONE',  ( 1.859271017917182139E-15, 26.18124999877096570, 12.99999999999999289 ) ) ;
#8975 = EDGE_LOOP ( 'NONE', ( #8546, #2393 ) ) ;
#8976 = CARTESIAN_POINT ( 'NONE',  ( -1.071796769724488563, 25.76740381056766793, 12.99999999999999289 ) ) ;
#8977 = EDGE_CURVE ( 'NONE', #8256, #20149, #7822, .T. ) ;
#8978 = CARTESIAN_POINT ( 'NONE',  ( -11.91206721063010754, 28.72825533807145959, -2.750000000000000000 ) ) ;
#8979 = CARTESIAN_POINT ( 'NONE',  ( 6.009258394948636914E-15, 26.15312499938548640, 4.662447845253954171 ) ) ;
#8980 = DIRECTION ( 'NONE',  ( 0.000000000000000000, 1.000000000000000000, 0.000000000000000000 ) ) ;
#8981 = CARTESIAN_POINT ( 'NONE',  ( 2.000000000000000000, 25.37500000000000355, 12.46410161513774817 ) ) ;
#8982 = CARTESIAN_POINT ( 'NONE',  ( 1.071796769724491671, 28.90134618820330559, 12.99999999999999467 ) ) ;
#8983 = CARTESIAN_POINT ( 'NONE',  ( 1.071796769724487230, -28.28259618943233988, 4.999999999999992006 ) ) ;
#8984 = DIRECTION ( 'NONE',  ( 0.000000000000000000, 0.000000000000000000, 1.000000000000000000 ) ) ;
#8985 = CARTESIAN_POINT ( 'NONE',  ( 1.878215178125004048, 27.91562499938548569, 5.746835883940462963 ) ) ;
#8986 = CARTESIAN_POINT ( 'NONE',  ( -7.234255490826573265, 30.12293631110053838, -6.500000000000000000 ) ) ;
#8987 = CARTESIAN_POINT ( 'NONE',  ( 20.82429470594385634, 15.16744045645140915, 8.999999999999992895 ) ) ;
#8988 = CARTESIAN_POINT ( 'NONE',  ( 15.70427213685309020, 21.01666689277176658, 11.16877607737301226 ) ) ;
#8989 = CARTESIAN_POINT ( 'NONE',  ( 0.000000000000000000, 0.000000000000000000, 1.000000000000000000 ) ) ;
#8990 = CARTESIAN_POINT ( 'NONE',  ( 1.878215178125000939, 26.86562499938548498, 12.25316411605952283 ) ) ;
#8991 = CARTESIAN_POINT ( 'NONE',  ( -3.110308778861381462, 34.50000000000000000, 3.869115154270378110 ) ) ;
#8992 = CARTESIAN_POINT ( 'NONE',  ( 17.21571288163933033, 22.52810763755800494, 11.16877607737301048 ) ) ;
#8993 = ORIENTED_EDGE ( 'NONE', *, *, #3561, .F. ) ;
#8994 = CARTESIAN_POINT ( 'NONE',  ( 3.897863563849872204, 30.85476721088026508, -6.500000000000000000 ) ) ;
#8995 = CARTESIAN_POINT ( 'NONE',  ( -1.999999999999995781, 28.24374999877096570, 5.535898384862237620 ) ) ;
#8996 = CARTESIAN_POINT ( 'NONE',  ( -3.756430356250003655, -27.84062499938548640, 8.999999999999992895 ) ) ;
#8998 = ORIENTED_EDGE ( 'NONE', *, *, #8254, .T. ) ;
#8997 = FACE_OUTER_BOUND ( 'NONE', #14691, .T. ) ;
#8999 = CARTESIAN_POINT ( 'NONE',  ( -25.98730014090454432, -17.08421000182750760, 1.000000000000000000 ) ) ;
#9000 = EDGE_CURVE ( 'NONE', #15395, #12207, #25870, .T. ) ;
#9001 = EDGE_LOOP ( 'NONE', ( #2065, #11333, #20394, #11800 ) ) ;
#9002 = CARTESIAN_POINT ( 'NONE',  ( 1.878215178124995832, -27.54062499938548214, 5.746835883940462963 ) ) ;
#9003 = VERTEX_POINT ( 'NONE', #21948 ) ;
#9004 = VERTEX_POINT ( 'NONE', #4027 ) ;
#9005 = EDGE_CURVE ( 'NONE', #13593, #16478, #1904, .T. ) ;
#9006 = CARTESIAN_POINT ( 'NONE',  ( 19.41874785118199043, 22.86831248503511205, 5.819033386899013394 ) ) ;
#9007 = CARTESIAN_POINT ( 'NONE',  ( -3.756430356250000546, 28.21562499938548640, 11.16877607737301226 ) ) ;
#9008 = EDGE_CURVE ( 'NONE', #17868, #2787, #11695, .T. ) ;
#9009 = CARTESIAN_POINT ( 'NONE',  ( 1.859271017917182139E-15, 28.88124999877096499, 12.99999999999999289 ) ) ;
#9010 = CARTESIAN_POINT ( 'NONE',  ( -3.027295627619581708, 38.86045373840903494, 4.241260441470868336 ) ) ;
#9011 = CARTESIAN_POINT ( 'NONE',  ( 3.756430356250002323, 28.25312499938548427, 11.16877607737301226 ) ) ;
#9012 = CYLINDRICAL_SURFACE ( 'NONE', #1289, 31.10000000000000142 ) ;
#9013 = LINE ( 'NONE', #12936, #11713 ) ;
#9014 = FACE_OUTER_BOUND ( 'NONE', #12797, .T. ) ;
#9015 = SURFACE_SIDE_STYLE ('',( #4957 ) ) ;
#9016 = DIRECTION ( 'NONE',  ( 1.000000000000000000, 0.000000000000000000, 0.000000000000000000 ) ) ;
#9017 = CARTESIAN_POINT ( 'NONE',  ( -9.133673601486680838, -29.72853858738275434, -6.500000000000000000 ) ) ;
#9018 = CARTESIAN_POINT ( 'NONE',  ( 1.878215178124995832, -28.10312499938548569, 5.746835883940462963 ) ) ;
#9019 = DIRECTION ( 'NONE',  ( 0.000000000000000000, 0.000000000000000000, 1.000000000000000000 ) ) ;
#9020 = CARTESIAN_POINT ( 'NONE',  ( -30.12293631110050995, -7.734255490826679846, -6.500000000000000000 ) ) ;
#9021 = CARTESIAN_POINT ( 'NONE',  ( -17.87326343783962201, -25.45105997952905597, -2.750000000000000000 ) ) ;
#9022 = LINE ( 'NONE', #1304, #21427 ) ;
#9023 = ORIENTED_EDGE ( 'NONE', *, *, #11186, .T. ) ;
#9024 = DIRECTION ( 'NONE',  ( 0.000000000000000000, -1.000000000000000000, 0.000000000000000000 ) ) ;
#9026 = EDGE_LOOP ( 'NONE', ( #21156, #17034, #6961, #16298 ) ) ;
#9025 = DIRECTION ( 'NONE',  ( 1.000000000000000000, 0.000000000000000000, 0.000000000000000000 ) ) ;
#9027 = ORIENTED_EDGE ( 'NONE', *, *, #13139, .F. ) ;
#9028 = ORIENTED_EDGE ( 'NONE', *, *, #208, .T. ) ;
#9029 = ORIENTED_EDGE ( 'NONE', *, *, #1068, .T. ) ;
#9030 = VERTEX_POINT ( 'NONE', #24298 ) ;
#9031 = DIRECTION ( 'NONE',  ( 0.000000000000000000, 0.000000000000000000, -1.000000000000000000 ) ) ;
#9032 = CARTESIAN_POINT ( 'NONE',  ( 22.67092431280578779, -21.28941499438234786, -6.500000000000000000 ) ) ;
#9033 =( BOUNDED_CURVE ( )  B_SPLINE_CURVE ( 2, ( #3744, #10143, #17618, #1925, #15536, #1801, #4005, #23503, #22042 ),
 .UNSPECIFIED., .F., .F. ) 
 B_SPLINE_CURVE_WITH_KNOTS ( ( 3, 2, 2, 2, 3 ),
 ( 0.1749999999999999889, 0.1833333333333333204, 0.2000000000000000111, 0.2166666666666666741, 0.2250000000000000056 ),
 .UNSPECIFIED. ) 
 CURVE ( )  GEOMETRIC_REPRESENTATION_ITEM ( )  RATIONAL_B_SPLINE_CURVE ( ( 0.9330127018922194093, 0.9330127018922194093, 1.000000000000000000, 0.8660254037844387076, 1.000000000000000000, 0.8660254037844387076, 1.000000000000000000, 0.9330127018922194093, 0.9330127018922194093 ) ) 
 REPRESENTATION_ITEM ( '' )  );
#9034 = ORIENTED_EDGE ( 'NONE', *, *, #2689, .F. ) ;
#9035 = EDGE_CURVE ( 'NONE', #1175, #24947, #12267, .T. ) ;
#9036 = CARTESIAN_POINT ( 'NONE',  ( -3.756430356249996994, 29.07812499938548356, 8.999999999999992895 ) ) ;
#9037 = EDGE_CURVE ( 'NONE', #13915, #130, #24158, .T. ) ;
#9038 = CARTESIAN_POINT ( 'NONE',  ( 3.756430356250002323, -11.16877607737301226, 1.003124999385480276 ) ) ;
#9039 =( LENGTH_UNIT ( ) NAMED_UNIT ( * ) SI_UNIT ( .MILLI., .METRE. ) );
#9040 = CARTESIAN_POINT ( 'NONE',  ( 23.58876780933789519, 18.27637305341907492, 11.16877607737301226 ) ) ;
#9041 = EDGE_CURVE ( 'NONE', #9149, #20576, #4682, .T. ) ;
#9042 = CARTESIAN_POINT ( 'NONE',  ( -1.878215178124998497, 26.90312499938548285, 12.25316411605951927 ) ) ;
#9043 = CARTESIAN_POINT ( 'NONE',  ( 15.85973458909327505, -20.67279826512041296, 20.00001199999999457 ) ) ;
#9044 = CARTESIAN_POINT ( 'NONE',  ( -3.756430356249995661, -6.831223922626973533, 3.928124999385480542 ) ) ;
#9045 = FACE_OUTER_BOUND ( 'NONE', #20329, .T. ) ;
#9046 = CARTESIAN_POINT ( 'NONE',  ( 24.86329371854774806, 18.68225429291723216, 1.000000000000000000 ) ) ;
#9047 = CARTESIAN_POINT ( 'NONE',  ( -3.834746474454188013E-15, -28.20624999877096428, 4.999999999999992006 ) ) ;
#9048 = CARTESIAN_POINT ( 'NONE',  ( 31.00322564728513086, -2.451530025009243108, -2.750000000000000000 ) ) ;
#9049 = CARTESIAN_POINT ( 'NONE',  ( 1.878215178125000939, -12.25316411605952283, 3.778124999385484628 ) ) ;
#9050 = CARTESIAN_POINT ( 'NONE',  ( 0.000000000000000000, 0.000000000000000000, 1.000000000000000000 ) ) ;
#9051 = DIRECTION ( 'NONE',  ( 0.000000000000000000, 0.000000000000000000, -1.000000000000000000 ) ) ;
#9052 = ORIENTED_EDGE ( 'NONE', *, *, #6163, .T. ) ;
#9053 = VERTEX_POINT ( 'NONE', #6384 ) ;
#9054 = ORIENTED_EDGE ( 'NONE', *, *, #16182, .T. ) ;
#9055 = CARTESIAN_POINT ( 'NONE',  ( 0.000000000000000000, 10.00000000000000000, 15.00000000000000178 ) ) ;
#9056 = ORIENTED_EDGE ( 'NONE', *, *, #15274, .T. ) ;
#9057 = CARTESIAN_POINT ( 'NONE',  ( -3.735045420075836212E-15, -25.81562499938548783, 4.662447845253954171 ) ) ;
#9058 = ORIENTED_EDGE ( 'NONE', *, *, #25170, .F. ) ;
#9059 = CARTESIAN_POINT ( 'NONE',  ( -1.071796769724482123, 27.96115380933863648, 12.99999999999999645 ) ) ;
#9060 = EDGE_CURVE ( 'NONE', #14404, #9218, #4296, .T. ) ;
#9061 = VERTEX_POINT ( 'NONE', #248 ) ;
#9062 = CARTESIAN_POINT ( 'NONE',  ( -13.24173596767339767, 28.14012133169338270, -6.500000000000000000 ) ) ;
#9063 = CARTESIAN_POINT ( 'NONE',  ( -1.999999999999995781, 25.15000000000000213, 5.535898384862237620 ) ) ;
#9064 = CARTESIAN_POINT ( 'NONE',  ( 18.28634663658058912, 19.80209616443256593, 4.999999999999992895 ) ) ;
#9065 = ADVANCED_FACE ( 'NONE', ( #8217 ), #18283, .F. ) ;
#9066 = DIRECTION ( 'NONE',  ( 0.000000000000000000, -0.000000000000000000, 1.000000000000000000 ) ) ;
#9067 = DIRECTION ( 'NONE',  ( 0.7071067811865487940, 0.7071067811865463515, 0.000000000000000000 ) ) ;
#9068 = CARTESIAN_POINT ( 'NONE',  ( 21.12273290994980712, 15.81033815403099752, 11.16877607737301226 ) ) ;
#9069 = CYLINDRICAL_SURFACE ( 'NONE', #10026, 4.000000000000000000 ) ;
#9070 = CARTESIAN_POINT ( 'NONE',  ( -1.999999999999995781, 25.60000000000000142, 5.535898384862237620 ) ) ;
#9071 =( BOUNDED_CURVE ( )  B_SPLINE_CURVE ( 2, ( #954, #1337, #1462, #1192, #23171, #5251, #6956, #14936, #11252 ),
 .UNSPECIFIED., .F., .F. ) 
 B_SPLINE_CURVE_WITH_KNOTS ( ( 3, 2, 2, 2, 3 ),
 ( 0.7249999999999999778, 0.7333333333333332815, 0.7500000000000000000, 0.7666666666666667185, 0.7750000000000000222 ),
 .UNSPECIFIED. ) 
 CURVE ( )  GEOMETRIC_REPRESENTATION_ITEM ( )  RATIONAL_B_SPLINE_CURVE ( ( 0.9330127018922194093, 0.9330127018922194093, 1.000000000000000000, 0.8660254037844387076, 1.000000000000000000, 0.8660254037844387076, 1.000000000000000000, 0.9330127018922194093, 0.9330127018922194093 ) ) 
 REPRESENTATION_ITEM ( '' )  );
#9072 = EDGE_CURVE ( 'NONE', #18519, #20151, #22982, .T. ) ;
#9073 = CARTESIAN_POINT ( 'NONE',  ( 17.26874589022832751, 22.58114064614699856, 8.999999999999992895 ) ) ;
#9074 = FACE_OUTER_BOUND ( 'NONE', #12132, .T. ) ;
#9075 = ORIENTED_EDGE ( 'NONE', *, *, #12648, .T. ) ;
#9076 = CARTESIAN_POINT ( 'NONE',  ( -3.999999999999999556, 28.35624999877097707, 11.30940107675849404 ) ) ;
#9077 = CARTESIAN_POINT ( 'NONE',  ( -3.756430356250003655, -27.84062499938548640, 8.999999999999992895 ) ) ;
#9078 = FACE_OUTER_BOUND ( 'NONE', #9251, .T. ) ;
#9079 = CARTESIAN_POINT ( 'NONE',  ( -3.756430356249995661, 27.69062499938548427, 6.831223922626973533 ) ) ;
#9080 = CARTESIAN_POINT ( 'NONE',  ( -3.469446951953614189E-15, -30.00000000000000355, 4.999999999999992006 ) ) ;
#9082 = VERTEX_POINT ( 'NONE', #2451 ) ;
#9081 = CARTESIAN_POINT ( 'NONE',  ( -1.878215178124995832, -5.746835883940462963, 0.2906249993854838065 ) ) ;
#9083 = ORIENTED_EDGE ( 'NONE', *, *, #4278, .F. ) ;
#9084 = DIRECTION ( 'NONE',  ( 1.000000000000000000, 0.000000000000000000, 0.000000000000000000 ) ) ;
#9085 = CYLINDRICAL_SURFACE ( 'NONE', #18846, 4.000000000000000000 ) ;
#9086 = ORIENTED_EDGE ( 'NONE', *, *, #8699, .F. ) ;
#9087 = CARTESIAN_POINT ( 'NONE',  ( 3.756430356249997438, -29.56562499938549493, 11.16877607737301048 ) ) ;
#9088 = LINE ( 'NONE', #8843, #24740 ) ;
#9089 = DIRECTION ( 'NONE',  ( 1.000000000000000000, 0.000000000000000000, 0.000000000000000000 ) ) ;
#9090 = CARTESIAN_POINT ( 'NONE',  ( -2.000000000000003997, -26.36874999877096926, 5.535898384862238508 ) ) ;
#9091 = CARTESIAN_POINT ( 'NONE',  ( 3.756430356250006319, 28.77812499938548640, 6.831223922626973533 ) ) ;
#9092 = EDGE_CURVE ( 'NONE', #20170, #25112, #24275, .T. ) ;
#9093 = CARTESIAN_POINT ( 'NONE',  ( -5.327558883616270613, -30.54913349766217934, -6.500000000000000000 ) ) ;
#9094 = PRODUCT_CONTEXT ( 'NONE', #3751, 'mechanical' ) ;
#9095 = CARTESIAN_POINT ( 'NONE',  ( -3.999999999999995559, 26.98750000000000071, 6.690598923241487306 ) ) ;
#9096 = CYLINDRICAL_SURFACE ( 'NONE', #19671, 4.000000000000000000 ) ;
#9097 = AXIS2_PLACEMENT_3D ( 'NONE', #13881, #9437, #15834 ) ;
#9098 = CARTESIAN_POINT ( 'NONE',  ( -1.878215178124998497, 26.79062499938548214, 12.25316411605951927 ) ) ;
#9099 = CARTESIAN_POINT ( 'NONE',  ( -5.706339097770935176, 29.50000000000000000, 7.645898033750358813 ) ) ;
#9100 = CARTESIAN_POINT ( 'NONE',  ( 18.07541709408115693, 18.07541709408108943, 4.381197846482986158 ) ) ;
#9101 = CARTESIAN_POINT ( 'NONE',  ( 18.09530447186750024, 18.09530447186743629, 13.33755215474602984 ) ) ;
#9102 = CARTESIAN_POINT ( 'NONE',  ( 3.735045420075836212E-15, 27.05312499938548498, 4.662447845253954171 ) ) ;
#9103 = CARTESIAN_POINT ( 'NONE',  ( 23.83637464252882765, 18.21619809234428189, 8.475804415688520166 ) ) ;
#9104 = CARTESIAN_POINT ( 'NONE',  ( 17.93393197184562027, 20.59012934980492560, 12.25316411605951927 ) ) ;
#9105 = CARTESIAN_POINT ( 'NONE',  ( 23.62178590814407642, 17.96493165865162212, 11.30940107675849760 ) ) ;
#9106 = AXIS2_PLACEMENT_3D ( 'NONE', #20134, #9934, #25645 ) ;
#9107 = VERTEX_POINT ( 'NONE', #2714 ) ;
#9108 = CARTESIAN_POINT ( 'NONE',  ( 1.859271017917182139E-15, 28.93749999999999645, 12.99999999999999289 ) ) ;
#9109 = CARTESIAN_POINT ( 'NONE',  ( 3.752267015613588906E-15, 28.65624999877096712, 4.381197846482986158 ) ) ;
#9110 = CARTESIAN_POINT ( 'NONE',  ( -4.000000000000001776, -25.41250000000000142, 11.30940107675849760 ) ) ;
#9112 = ORIENTED_EDGE ( 'NONE', *, *, #10025, .F. ) ;
#9111 = DIRECTION ( 'NONE',  ( 1.000000000000000000, 0.000000000000000000, 0.000000000000000000 ) ) ;
#9113 = CARTESIAN_POINT ( 'NONE',  ( 3.756430356250003655, 26.15312499938548640, 8.999999999999992895 ) ) ;
#9114 = ORIENTED_EDGE ( 'NONE', *, *, #19557, .F. ) ;
#9115 = CARTESIAN_POINT ( 'NONE',  ( 1.878215178124995832, -28.44062499938548427, 5.746835883940462963 ) ) ;
#9116 = ORIENTED_EDGE ( 'NONE', *, *, #23564, .F. ) ;
#9117 = ORIENTED_EDGE ( 'NONE', *, *, #1174, .F. ) ;
#9118 = CARTESIAN_POINT ( 'NONE',  ( 18.19529158423879878, 23.85228215861205570, 9.259737768674039415 ) ) ;
#9119 = CARTESIAN_POINT ( 'NONE',  ( 1.878215178124999829, 28.32812499938549422, 12.25316411605952283 ) ) ;
#9120 = AXIS2_PLACEMENT_3D ( 'NONE', #16101, #12416, #6662 ) ;
#9121 = CIRCLE ( 'NONE', #22076, 0.5000000000000005551 ) ;
#9122 = CARTESIAN_POINT ( 'NONE',  ( 3.735045420075836212E-15, -4.662447845253954171, 0.2531249993854848279 ) ) ;
#9123 = CIRCLE ( 'NONE', #8710, 0.5000000000000001110 ) ;
#9124 = EDGE_CURVE ( 'NONE', #961, #19280, #4558, .T. ) ;
#9125 = AXIS2_PLACEMENT_3D ( 'NONE', #7606, #5379, #6862 ) ;
#9126 = CARTESIAN_POINT ( 'NONE',  ( 3.834746474454188013E-15, 27.81249999999999645, 4.999999999999992006 ) ) ;
#9127 = DIRECTION ( 'NONE',  ( 0.000000000000000000, 0.000000000000000000, -1.000000000000000000 ) ) ;
#9128 = ADVANCED_FACE ( 'NONE', ( #12131 ), #6627, .T. ) ;
#9129 = DIRECTION ( 'NONE',  ( -1.000000000000000000, 0.000000000000000000, 0.000000000000000000 ) ) ;
#9130 = DIRECTION ( 'NONE',  ( 0.000000000000000000, -1.000000000000000000, 0.000000000000000000 ) ) ;
#9131 = UNCERTAINTY_MEASURE_WITH_UNIT (LENGTH_MEASURE( 1.000000000000000082E-05 ), #77, 'distance_accuracy_value', 'NONE');
#9132 = CARTESIAN_POINT ( 'NONE',  ( 1.878215178125004048, 28.81562499938548427, 5.746835883940462963 ) ) ;
#9133 = DIRECTION ( 'NONE',  ( 0.000000000000000000, -1.000000000000000000, 0.000000000000000000 ) ) ;
#9134 = DIRECTION ( 'NONE',  ( 0.000000000000000000, 0.000000000000000000, 1.000000000000000000 ) ) ;
#9135 = CARTESIAN_POINT ( 'NONE',  ( -30.12293631110035363, 7.734255490827311341, -6.500000000000000000 ) ) ;
#9136 = EDGE_CURVE ( 'NONE', #17175, #15910, #8090, .T. ) ;
#9137 = CARTESIAN_POINT ( 'NONE',  ( -7.734255490827218971, -30.12293631110037140, -6.500000000000000000 ) ) ;
#9138 = CARTESIAN_POINT ( 'NONE',  ( -30.04913349766215802, 5.827558883616378083, -6.500000000000000000 ) ) ;
#9139 = CARTESIAN_POINT ( 'NONE',  ( -1.878215178124998497, 26.45312499938548711, 12.25316411605951927 ) ) ;
#9140 = DIRECTION ( 'NONE',  ( 0.000000000000000000, 0.000000000000000000, -1.000000000000000000 ) ) ;
#9141 = VECTOR ( 'NONE', #16372, 1000.000000000000000 ) ;
#9142 = CARTESIAN_POINT ( 'NONE',  ( -13.24173596767398742, -28.14012133169310559, 1.000000000000000000 ) ) ;
#9143 = CARTESIAN_POINT ( 'NONE',  ( -3.959305739469038251E-15, -30.00000000000000355, 12.99999999999999289 ) ) ;
#9145 = ORIENTED_EDGE ( 'NONE', *, *, #14033, .F. ) ;
#9144 = CIRCLE ( 'NONE', #382, 31.10000000000000142 ) ;
#9146 = EDGE_CURVE ( 'NONE', #10041, #16921, #2949, .T. ) ;
#9147 = CARTESIAN_POINT ( 'NONE',  ( 3.526711513754847704, 31.50000000000000000, 13.85410196624967405 ) ) ;
#9149 = VERTEX_POINT ( 'NONE', #2837 ) ;
#9148 = DIRECTION ( 'NONE',  ( 0.000000000000000000, -0.000000000000000000, 1.000000000000000000 ) ) ;
#9150 =( BOUNDED_CURVE ( )  B_SPLINE_CURVE ( 2, ( #11120, #12833, #20807, #2890, #19099 ),
 .UNSPECIFIED., .F., .F. ) 
 B_SPLINE_CURVE_WITH_KNOTS ( ( 3, 2, 3 ),
 ( 0.9749999999999999778, 0.9833333333333332815, 1.000000000000000000 ),
 .UNSPECIFIED. ) 
 CURVE ( )  GEOMETRIC_REPRESENTATION_ITEM ( )  RATIONAL_B_SPLINE_CURVE ( ( 0.9330127018922194093, 0.9330127018922194093, 1.000000000000000000, 0.8660254037844387076, 1.000000000000000000 ) ) 
 REPRESENTATION_ITEM ( '' )  );
#9151 = AXIS2_PLACEMENT_3D ( 'NONE', #19146, #25181, #23331 ) ;
#9152 = ORIENTED_EDGE ( 'NONE', *, *, #25260, .T. ) ;
#9154 = VERTEX_POINT ( 'NONE', #885 ) ;
#9153 = AXIS2_PLACEMENT_3D ( 'NONE', #15682, #22208, #5862 ) ;
#9155 = ORIENTED_EDGE ( 'NONE', *, *, #2241, .F. ) ;
#9156 = ORIENTED_EDGE ( 'NONE', *, *, #6865, .T. ) ;
#9157 = CARTESIAN_POINT ( 'NONE',  ( 0.000000000000000000, 0.000000000000000000, 1.000000000000000000 ) ) ;
#9158 = DIRECTION ( 'NONE',  ( -1.000000000000000000, 0.000000000000000000, 0.000000000000000000 ) ) ;
#9159 = CARTESIAN_POINT ( 'NONE',  ( 1.500000000000001776, -10.49999999999999289, 4.999999999999993783 ) ) ;
#9160 = AXIS2_PLACEMENT_3D ( 'NONE', #22214, #2217, #10174 ) ;
#9161 = CARTESIAN_POINT ( 'NONE',  ( -3.756430356249995661, -6.831223922626973533, 4.490624999385484095 ) ) ;
#9162 = CARTESIAN_POINT ( 'NONE',  ( -3.999999999999996447, -8.999999999999992895, 1.968749998770967569 ) ) ;
#9163 = CARTESIAN_POINT ( 'NONE',  ( 19.41885621233737069, 22.07505359029666536, 5.746835883940462963 ) ) ;
#9164 = CARTESIAN_POINT ( 'NONE',  ( -3.469446951953614189E-15, -30.00000000000000355, 8.999999999999992895 ) ) ;
#9165 = AXIS2_PLACEMENT_3D ( 'NONE', #21491, #9199, #7625 ) ;
#9166 = DIRECTION ( 'NONE',  ( 1.000000000000000000, 0.000000000000000000, 0.000000000000000000 ) ) ;
#9167 = CARTESIAN_POINT ( 'NONE',  ( 18.15054718871317974, 23.80740143820548482, 8.999999999999992895 ) ) ;
#9168 = VECTOR ( 'NONE', #3458, 1000.000000000000000 ) ;
#9169 = CARTESIAN_POINT ( 'NONE',  ( 3.756430356250003655, -8.999999999999992895, 4.640624999385483562 ) ) ;
#9170 = CARTESIAN_POINT ( 'NONE',  ( -23.96296185032722548, -19.82388608118403539, -6.500000000000000000 ) ) ;
#9171 = DIRECTION ( 'NONE',  ( 1.000000000000000000, 0.000000000000000000, 0.000000000000000000 ) ) ;
#9172 = CARTESIAN_POINT ( 'NONE',  ( -4.000000000000003553, -29.50000000000000355, 8.999999999999992895 ) ) ;
#9173 = EDGE_CURVE ( 'NONE', #8491, #17932, #10743, .T. ) ;
#9174 = CARTESIAN_POINT ( 'NONE',  ( 1.999999999999995781, -25.54374999877096997, 5.535898384862237620 ) ) ;
#9175 = CARTESIAN_POINT ( 'NONE',  ( 3.756430356250003655, -8.999999999999992895, 4.753124999385485161 ) ) ;
#9176 = CARTESIAN_POINT ( 'NONE',  ( 3.999999999999997335, -26.61250000000000071, 11.30940107675849404 ) ) ;
#9177 = CARTESIAN_POINT ( 'NONE',  ( 3.469446951953614189E-15, 25.00000000000000000, 8.999999999999992895 ) ) ;
#9178 = ORIENTED_EDGE ( 'NONE', *, *, #8645, .F. ) ;
#9179 = ADVANCED_FACE ( 'NONE', ( #22732 ), #22984, .F. ) ;
#9180 = CARTESIAN_POINT ( 'NONE',  ( 0.000000000000000000, 0.000000000000000000, 19.50000000000000000 ) ) ;
#9181 = ORIENTED_EDGE ( 'NONE', *, *, #24234, .F. ) ;
#9182 = AXIS2_PLACEMENT_3D ( 'NONE', #2437, #14603, #8854 ) ;
#9183 = EDGE_CURVE ( 'NONE', #21627, #24890, #18384, .T. ) ;
#9185 = ORIENTED_EDGE ( 'NONE', *, *, #16833, .T. ) ;
#9184 = VECTOR ( 'NONE', #21151, 1000.000000000000000 ) ;
#9186 = CARTESIAN_POINT ( 'NONE',  ( 4.000000000000003553, -8.999999999999992895, 6.000000000000000000 ) ) ;
#9187 = ORIENTED_EDGE ( 'NONE', *, *, #15864, .F. ) ;
#9188 = CARTESIAN_POINT ( 'NONE',  ( 3.756430356249995661, -26.79062499938548925, 6.831223922626973533 ) ) ;
#9189 = VERTEX_POINT ( 'NONE', #21269 ) ;
#9190 = LINE ( 'NONE', #21485, #11772 ) ;
#9191 = VECTOR ( 'NONE', #683, 1000.000000000000000 ) ;
#9192 = AXIS2_PLACEMENT_3D ( 'NONE', #12206, #187, #4478 ) ;
#9193 = ORIENTED_EDGE ( 'NONE', *, *, #22721, .F. ) ;
#9194 = CARTESIAN_POINT ( 'NONE',  ( 21.21320343559646915, 21.21320343559638744, 12.99999999999999289 ) ) ;
#9195 = CARTESIAN_POINT ( 'NONE',  ( 2.672651547586948120E-15, 28.62812499938548783, 13.33755215474602984 ) ) ;
#9196 = DIRECTION ( 'NONE',  ( 0.000000000000000000, 0.000000000000000000, 1.000000000000000000 ) ) ;
#9197 = CIRCLE ( 'NONE', #14219, 0.5000000000000005551 ) ;
#9198 = DIRECTION ( 'NONE',  ( 0.000000000000000000, 1.000000000000000000, 0.000000000000000000 ) ) ;
#9199 = DIRECTION ( 'NONE',  ( -0.000000000000000000, -0.000000000000000000, 1.000000000000000000 ) ) ;
#9200 = CARTESIAN_POINT ( 'NONE',  ( 20.82877788845545552, 18.17258051049600454, 5.746835883940462963 ) ) ;
#9201 = AXIS2_PLACEMENT_3D ( 'NONE', #7600, #7341, #19366 ) ;
#9202 = CARTESIAN_POINT ( 'NONE',  ( -3.999999999999995559, 28.33750000000000213, 6.690598923241487306 ) ) ;
#9203 = AXIS2_PLACEMENT_3D ( 'NONE', #25709, #20842, #25403 ) ;
#9204 = CARTESIAN_POINT ( 'NONE',  ( 2.620986760973688460E-15, 25.33750000000000568, 13.61880215351699874 ) ) ;
#9205 = AXIS2_PLACEMENT_3D ( 'NONE', #21578, #25257, #3409 ) ;
#9206 = CARTESIAN_POINT ( 'NONE',  ( 22.07732706455164617, 16.76493230863282591, 11.16877607737301403 ) ) ;
#9207 = DIRECTION ( 'NONE',  ( 0.9980267284282724471, 0.06279051952930156388, 0.000000000000000000 ) ) ;
#9208 = EDGE_CURVE ( 'NONE', #25179, #1141, #13795, .T. ) ;
#9209 = ORIENTED_EDGE ( 'NONE', *, *, #6525, .T. ) ;
#9210 = ORIENTED_EDGE ( 'NONE', *, *, #7623, .F. ) ;
#9211 = CARTESIAN_POINT ( 'NONE',  ( 6.009258394948636914E-15, 27.75624999877097920, 4.381197846482986158 ) ) ;
#9213 = EDGE_CURVE ( 'NONE', #21597, #6260, #21026, .T. ) ;
#9212 = CARTESIAN_POINT ( 'NONE',  ( 3.756430356249996994, -29.41562499938548569, 8.999999999999992895 ) ) ;
#9214 = CARTESIAN_POINT ( 'NONE',  ( -29.09636799667067564, 10.98232076577254368, 1.000000000000000000 ) ) ;
#9215 = VECTOR ( 'NONE', #21800, 1000.000000000000000 ) ;
#9216 = CARTESIAN_POINT ( 'NONE',  ( -3.756430356249995661, 26.79062499938548925, 6.831223922626973533 ) ) ;
#9217 = PLANE ( 'NONE',  #23808 ) ;
#9218 = VERTEX_POINT ( 'NONE', #4811 ) ;
#9219 = ORIENTED_EDGE ( 'NONE', *, *, #7590, .F. ) ;
#9220 = CARTESIAN_POINT ( 'NONE',  ( 0.000000000000000000, 0.000000000000000000, 1.000000000000000000 ) ) ;
#9221 = AXIS2_PLACEMENT_3D ( 'NONE', #13700, #7562, #25231 ) ;
#9222 = CIRCLE ( 'NONE', #15904, 31.10000000000000142 ) ;
#9223 = CARTESIAN_POINT ( 'NONE',  ( 0.000000000000000000, 0.000000000000000000, -6.500000000000000000 ) ) ;
#9224 = ORIENTED_EDGE ( 'NONE', *, *, #4278, .T. ) ;
#9225 = AXIS2_PLACEMENT_3D ( 'NONE', #6873, #22831, #7265 ) ;
#9226 = CARTESIAN_POINT ( 'NONE',  ( -3.756430356250003655, -28.85312499938548569, 8.999999999999992895 ) ) ;
#9227 = CARTESIAN_POINT ( 'NONE',  ( 3.756430356250004987, 29.64062499938548711, 8.999999999999992895 ) ) ;
#9228 = CARTESIAN_POINT ( 'NONE',  ( 1.878215178125001605, 26.41562499938548925, 12.25316411605952283 ) ) ;
#9229 = CIRCLE ( 'NONE', #12567, 0.5000000000000007772 ) ;
#9230 = CARTESIAN_POINT ( 'NONE',  ( 20.41007196385330147, 18.89432243600117900, 4.999999999999992895 ) ) ;
#9231 = CARTESIAN_POINT ( 'NONE',  ( 1.878215178125001605, 29.11562499938549209, 12.25316411605952283 ) ) ;
#9232 =( BOUNDED_CURVE ( )  B_SPLINE_CURVE ( 2, ( #10253, #328, #16040, #18136, #20196 ),
 .UNSPECIFIED., .F., .F. ) 
 B_SPLINE_CURVE_WITH_KNOTS ( ( 3, 2, 3 ),
 ( 0.000000000000000000, 0.01666666666666666644, 0.02500000000000000486 ),
 .UNSPECIFIED. ) 
 CURVE ( )  GEOMETRIC_REPRESENTATION_ITEM ( )  RATIONAL_B_SPLINE_CURVE ( ( 1.000000000000000000, 0.8660254037844387076, 1.000000000000000000, 0.9330127018922194093, 0.9330127018922194093 ) ) 
 REPRESENTATION_ITEM ( '' )  );
#9233 = AXIS2_PLACEMENT_3D ( 'NONE', #4239, #20186, #12466 ) ;
#9234 = CARTESIAN_POINT ( 'NONE',  ( -3.999999999999996447, -8.999999999999992895, 2.024999999999999023 ) ) ;
#9235 = SHAPE_DEFINITION_REPRESENTATION ( #469, #1120 ) ;
#9236 = DIRECTION ( 'NONE',  ( -0.9510565162951518658, 0.3090169943749528914, 0.000000000000000000 ) ) ;
#9237 = AXIS2_PLACEMENT_3D ( 'NONE', #22203, #4290, #8336 ) ;
#9238 = AXIS2_PLACEMENT_3D ( 'NONE', #20221, #13835, #14225 ) ;
#9239 = FACE_OUTER_BOUND ( 'NONE', #7963, .T. ) ;
#9240 = CARTESIAN_POINT ( 'NONE',  ( 1.878215178125000939, 27.76562499938548356, 12.25316411605952283 ) ) ;
#9241 = CARTESIAN_POINT ( 'NONE',  ( -1.775433037296146654, -29.94838521766437722, 5.406171146379000092 ) ) ;
#9242 = CARTESIAN_POINT ( 'NONE',  ( 14.98182492639001673, 20.63867917588233070, 6.690598923241487306 ) ) ;
#9243 = CARTESIAN_POINT ( 'NONE',  ( 21.14924941424430571, 15.83685465832548900, 8.999999999999992895 ) ) ;
#9244 = EDGE_CURVE ( 'NONE', #12726, #1614, #20758, .T. ) ;
#9245 = CYLINDRICAL_SURFACE ( 'NONE', #12575, 4.000000000000000000 ) ;
#9246 = CARTESIAN_POINT ( 'NONE',  ( 2.672651547586948120E-15, 28.17812499938548143, 13.33755215474602984 ) ) ;
#9247 = VECTOR ( 'NONE', #12646, 1000.000000000000000 ) ;
#9248 = CARTESIAN_POINT ( 'NONE',  ( -1.394453263437886604E-15, 27.30624999877096926, 4.999999999999991118 ) ) ;
#9249 = CARTESIAN_POINT ( 'NONE',  ( 16.52628376998245230, 21.83867852590111980, 6.831223922626973533 ) ) ;
#9250 = CARTESIAN_POINT ( 'NONE',  ( -1.859271017917182139E-15, 26.46249999999999858, 4.999999999999991118 ) ) ;
#9251 = EDGE_LOOP ( 'NONE', ( #5739, #20270, #2150, #12563 ) ) ;
#9252 = CARTESIAN_POINT ( 'NONE',  ( 1.071796769724491227, 26.83615380933863293, 4.999999999999989342 ) ) ;
#9253 = CARTESIAN_POINT ( 'NONE',  ( -1.878215178124995832, 26.30312499938548498, 5.746835883940462963 ) ) ;
#9254 = CARTESIAN_POINT ( 'NONE',  ( 3.999999999999997335, -25.26249999999999929, 11.30940107675849404 ) ) ;
#9256 = ORIENTED_EDGE ( 'NONE', *, *, #19094, .F. ) ;
#9255 = FACE_OUTER_BOUND ( 'NONE', #24299, .T. ) ;
#9257 = CARTESIAN_POINT ( 'NONE',  ( -3.756430356249996994, 26.37812499938548783, 8.999999999999992895 ) ) ;
#9258 = EDGE_CURVE ( 'NONE', #18497, #1729, #15147, .T. ) ;
#9259 = VERTEX_POINT ( 'NONE', #2975 ) ;
#9260 = CARTESIAN_POINT ( 'NONE',  ( -2.672651547586948120E-15, -29.07812499938548001, 13.33755215474602984 ) ) ;
#9261 = EDGE_LOOP ( 'NONE', ( #21068, #5901, #20118, #13572 ) ) ;
#9262 = ORIENTED_EDGE ( 'NONE', *, *, #18674, .F. ) ;
#9263 = DIRECTION ( 'NONE',  ( 0.000000000000000000, 1.000000000000000000, 0.000000000000000000 ) ) ;
#9264 = AXIS2_PLACEMENT_3D ( 'NONE', #10293, #13981, #21950 ) ;
#9265 = CARTESIAN_POINT ( 'NONE',  ( 3.756430356250004543, 27.01562499938549067, 11.16877607737301226 ) ) ;
#9266 = EDGE_CURVE ( 'NONE', #9323, #8387, #7113, .T. ) ;
#9267 = CARTESIAN_POINT ( 'NONE',  ( 1.878215178125000939, -12.25316411605952283, 1.865624999385483873 ) ) ;
#9268 = AXIS2_PLACEMENT_3D ( 'NONE', #18632, #14333, #14714 ) ;
#9269 = CARTESIAN_POINT ( 'NONE',  ( 1.071796769724492338, 28.90134618820330203, 12.99999999999999467 ) ) ;
#9270 =( LENGTH_UNIT ( ) NAMED_UNIT ( * ) SI_UNIT ( .MILLI., .METRE. ) );
#9271 = CARTESIAN_POINT ( 'NONE',  ( 6.938893903907228378E-15, 29.50000000000000000, 2.999999999999992450 ) ) ;
#9272 = CYLINDRICAL_SURFACE ( 'NONE', #18007, 0.5000000000000001110 ) ;
#9273 = AXIS2_PLACEMENT_3D ( 'NONE', #10303, #12009, #22084 ) ;
#9274 = DIRECTION ( 'NONE',  ( 1.000000000000000000, 0.000000000000000000, 0.000000000000000000 ) ) ;
#9275 = CARTESIAN_POINT ( 'NONE',  ( -3.999999999999996447, -8.999999999999992895, 18.00000000000000000 ) ) ;
#9276 = DIRECTION ( 'NONE',  ( -0.3090169943749528914, -0.9510565162951518658, 0.000000000000000000 ) ) ;
#9277 = LINE ( 'NONE', #23141, #7876 ) ;
#9278 = PLANE ( 'NONE',  #14314 ) ;
#9279 = CARTESIAN_POINT ( 'NONE',  ( -1.071796769724492338, -29.80134618820330417, 12.99999999999999467 ) ) ;
#9280 = CARTESIAN_POINT ( 'NONE',  ( -3.756430356250003655, -29.30312499938548498, 8.999999999999992895 ) ) ;
#9281 = CIRCLE ( 'NONE', #4689, 5.000000000000000888 ) ;
#9282 = CARTESIAN_POINT ( 'NONE',  ( 20.10392967174102097, 20.10392967174092860, 12.99999999999999289 ) ) ;
#9283 = CIRCLE ( 'NONE', #10512, 31.10000000000000142 ) ;
#9284 = LINE ( 'NONE', #14911, #4964 ) ;
#9285 = DIRECTION ( 'NONE',  ( 1.000000000000000000, 0.000000000000000000, 0.000000000000000000 ) ) ;
#9286 = CARTESIAN_POINT ( 'NONE',  ( 1.039771317798496408, -29.98307469845295969, 12.87134967428165666 ) ) ;
#9287 = ORIENTED_EDGE ( 'NONE', *, *, #18776, .T. ) ;
#9288 = CARTESIAN_POINT ( 'NONE',  ( 4.000000000000003553, 27.28749999999999787, 6.690598923241489970 ) ) ;
#9289 = DIRECTION ( 'NONE',  ( -0.000000000000000000, -1.000000000000000000, -0.000000000000000000 ) ) ;
#9291 = ORIENTED_EDGE ( 'NONE', *, *, #21260, .T. ) ;
#9290 = DIRECTION ( 'NONE',  ( 1.000000000000000000, 0.000000000000000000, 0.000000000000000000 ) ) ;
#9293 = VERTEX_POINT ( 'NONE', #1132 ) ;
#9292 = EDGE_CURVE ( 'NONE', #10594, #2244, #19048, .T. ) ;
#9294 = EDGE_LOOP ( 'NONE', ( #12026, #11071, #898, #9634 ) ) ;
#9295 = EDGE_LOOP ( 'NONE', ( #1976, #13211, #15688, #23274, #10527, #14946, #25082, #12452, #14548, #5114, #10489, #8025, #13237, #19401, #23306, #5037, #4539, #13381, #9187, #1623, #3706, #3499, #12398, #763 ) ) ;
#9296 = ORIENTED_EDGE ( 'NONE', *, *, #3390, .F. ) ;
#9297 = CARTESIAN_POINT ( 'NONE',  ( 27.25313774936419620, 14.98253926456328244, -6.500000000000000000 ) ) ;
#9298 = DIRECTION ( 'NONE',  ( 0.000000000000000000, 1.000000000000000000, 0.000000000000000000 ) ) ;
#9299 = EDGE_CURVE ( 'NONE', #10227, #14283, #7248, .T. ) ;
#9300 = VECTOR ( 'NONE', #3532, 1000.000000000000000 ) ;
#9301 = CARTESIAN_POINT ( 'NONE',  ( 3.756430356250004987, 25.14062499938548356, 8.999999999999992895 ) ) ;
#9302 = AXIS2_PLACEMENT_3D ( 'NONE', #11400, #4999, #12981 ) ;
#9303 = CARTESIAN_POINT ( 'NONE',  ( 3.735045420075836212E-15, -4.662447845253954171, 1.603124999385479921 ) ) ;
#9304 = CARTESIAN_POINT ( 'NONE',  ( -3.999999999999997335, -11.30940107675849404, 1.556249998770965037 ) ) ;
#9305 = CARTESIAN_POINT ( 'NONE',  ( -3.756430356249996994, 25.47812499938548569, 8.999999999999992895 ) ) ;
#9306 = CARTESIAN_POINT ( 'NONE',  ( -2.000000000000003997, -26.81874999877096855, 5.535898384862238508 ) ) ;
#9307 = CARTESIAN_POINT ( 'NONE',  ( 19.51172774249728192, 22.34015486724339183, 5.535898384862237620 ) ) ;
#9308 = CARTESIAN_POINT ( 'NONE',  ( 3.735045420075836212E-15, -4.662447845253954171, 3.403124999385483296 ) ) ;
#9309 = FACE_OUTER_BOUND ( 'NONE', #5198, .T. ) ;
#9310 = CARTESIAN_POINT ( 'NONE',  ( -13.24173596767339767, 28.14012133169338270, -6.500000000000000000 ) ) ;
#9311 = LINE ( 'NONE', #7343, #17625 ) ;
#9312 = CARTESIAN_POINT ( 'NONE',  ( 1.999999999999995781, -26.44374999877096855, 5.535898384862237620 ) ) ;
#9313 = CARTESIAN_POINT ( 'NONE',  ( -1.878215178124998497, -12.25316411605951927, 4.153124999385485516 ) ) ;
#9314 = LINE ( 'NONE', #17299, #15374 ) ;
#9315 = AXIS2_PLACEMENT_3D ( 'NONE', #1840, #11888, #9677 ) ;
#9316 = LINE ( 'NONE', #25266, #7469 ) ;
#9317 = CARTESIAN_POINT ( 'NONE',  ( 1.859271017917182139E-15, 25.78750000000000142, 12.99999999999999289 ) ) ;
#9318 = ORIENTED_EDGE ( 'NONE', *, *, #25140, .F. ) ;
#9319 = EDGE_CURVE ( 'NONE', #22273, #19788, #20907, .T. ) ;
#9320 = DIRECTION ( 'NONE',  ( 0.000000000000000000, 0.000000000000000000, 1.000000000000000000 ) ) ;
#9321 = VERTEX_POINT ( 'NONE', #9250 ) ;
#9322 = AXIS2_PLACEMENT_3D ( 'NONE', #16074, #1691, #11611 ) ;
#9323 = VERTEX_POINT ( 'NONE', #11715 ) ;
#9324 = DIRECTION ( 'NONE',  ( 0.000000000000000000, -0.000000000000000000, 1.000000000000000000 ) ) ;
#9325 = ORIENTED_EDGE ( 'NONE', *, *, #22246, .T. ) ;
#9326 = CARTESIAN_POINT ( 'NONE',  ( -3.735045420075836212E-15, -28.96562499938548640, 4.662447845253954171 ) ) ;
#9327 = VERTEX_POINT ( 'NONE', #25324 ) ;
#9328 = DIRECTION ( 'NONE',  ( 0.000000000000000000, 0.000000000000000000, -1.000000000000000000 ) ) ;
#9329 = EDGE_CURVE ( 'NONE', #1173, #5294, #9905, .T. ) ;
#9330 = AXIS2_PLACEMENT_3D ( 'NONE', #11273, #19257, #1357 ) ;
#9331 = VERTEX_POINT ( 'NONE', #11577 ) ;
#9332 = ADVANCED_FACE ( 'NONE', ( #23737 ), #19691, .T. ) ;
#9333 = CARTESIAN_POINT ( 'NONE',  ( -1.999999999999998224, 28.00000000000000000, 12.46410161513774639 ) ) ;
#9334 = DIRECTION ( 'NONE',  ( -1.000000000000000000, 2.891205793294678326E-16, 0.000000000000000000 ) ) ;
#9335 = CARTESIAN_POINT ( 'NONE',  ( 1.071796769724495668, 26.25759618943233065, 12.99999999999999112 ) ) ;
#9336 = DIRECTION ( 'NONE',  ( 0.000000000000000000, 0.000000000000000000, -1.000000000000000000 ) ) ;
#9337 = CARTESIAN_POINT ( 'NONE',  ( 16.66113976570983368, 19.31733714366914256, 12.25316411605951927 ) ) ;
#9338 = EDGE_CURVE ( 'NONE', #23470, #10871, #21727, .T. ) ;
#9339 = DIRECTION ( 'NONE',  ( 0.000000000000000000, 0.000000000000000000, 1.000000000000000000 ) ) ;
#9340 = CARTESIAN_POINT ( 'NONE',  ( -3.999999999999997335, 25.26249999999999929, 11.30940107675849404 ) ) ;
#9341 = CARTESIAN_POINT ( 'NONE',  ( 21.75912901301770219, 16.44673425709888548, 11.16877607737301403 ) ) ;
#9342 = DIRECTION ( 'NONE',  ( 0.000000000000000000, 1.000000000000000000, 0.000000000000000000 ) ) ;
#9343 = EDGE_CURVE ( 'NONE', #345, #23841, #24956, .T. ) ;
#9344 =( GEOMETRIC_REPRESENTATION_CONTEXT ( 3 ) GLOBAL_UNCERTAINTY_ASSIGNED_CONTEXT ( ( #20656 ) ) GLOBAL_UNIT_ASSIGNED_CONTEXT ( ( #24180, #6268, #3924 ) ) REPRESENTATION_CONTEXT ( 'NONE', 'WORKASPACE' ) );
#9345 = ORIENTED_EDGE ( 'NONE', *, *, #1634, .T. ) ;
#9346 = ORIENTED_EDGE ( 'NONE', *, *, #14439, .F. ) ;
#9347 = CARTESIAN_POINT ( 'NONE',  ( 4.000000000000001776, 27.19374999877097210, 8.999999999999992895 ) ) ;
#9348 = CARTESIAN_POINT ( 'NONE',  ( -1.878215178125004048, -29.26562499938548356, 5.746835883940462963 ) ) ;
#9349 = VECTOR ( 'NONE', #9393, 1000.000000000000000 ) ;
#9350 = ORIENTED_EDGE ( 'NONE', *, *, #20699, .T. ) ;
#9351 = CYLINDRICAL_SURFACE ( 'NONE', #5417, 0.7500000000000001110 ) ;
#9352 = CARTESIAN_POINT ( 'NONE',  ( 3.735045420075836212E-15, 28.51562499938549067, 4.662447845253954171 ) ) ;
#9353 = CARTESIAN_POINT ( 'NONE',  ( 3.063240906311874401, 29.84319947910909931, 11.57226653943513028 ) ) ;
#9354 = ORIENTED_EDGE ( 'NONE', *, *, #19887, .F. ) ;
#9355 = ORIENTED_EDGE ( 'NONE', *, *, #14577, .T. ) ;
#9356 = CARTESIAN_POINT ( 'NONE',  ( 3.469446951953614189E-15, 30.00000000000000355, 8.999999999999992895 ) ) ;
#9357 = CARTESIAN_POINT ( 'NONE',  ( 3.718542035834364277E-15, 25.11250000000000782, 4.999999999999992006 ) ) ;
#9358 = EDGE_LOOP ( 'NONE', ( #377, #15720 ) ) ;
#9359 = CARTESIAN_POINT ( 'NONE',  ( -3.756430356250003655, -29.75312499938548783, 8.999999999999992895 ) ) ;
#9360 = DIRECTION ( 'NONE',  ( 0.000000000000000000, -1.000000000000000000, 0.000000000000000000 ) ) ;
#9361 = CARTESIAN_POINT ( 'NONE',  ( 6.009258394948636914E-15, 27.95312499938548356, 4.662447845253954171 ) ) ;
#9362 = CARTESIAN_POINT ( 'NONE',  ( 30.12293631110045311, 7.734255490826897450, -6.500000000000000000 ) ) ;
#9363 = CARTESIAN_POINT ( 'NONE',  ( -3.756430356249997882, 29.41562499938548569, 8.999999999999992895 ) ) ;
#9364 = EDGE_CURVE ( 'NONE', #23065, #20357, #15527, .T. ) ;
#9365 = EDGE_CURVE ( 'NONE', #1139, #11943, #10439, .T. ) ;
#9366 = CARTESIAN_POINT ( 'NONE',  ( -30.00000000000000355, 0.000000000000000000, 20.00000000000000000 ) ) ;
#9367 = EDGE_CURVE ( 'NONE', #24860, #5409, #5445, .T. ) ;
#9368 = CARTESIAN_POINT ( 'NONE',  ( -28.41604871112448549, 11.44867358849382910, -6.500000000000000000 ) ) ;
#9369 = ADVANCED_FACE ( 'NONE', ( #25834 ), #17359, .F. ) ;
#9370 = CARTESIAN_POINT ( 'NONE',  ( -3.756430356249996994, 27.16562499938548214, 8.999999999999992895 ) ) ;
#9371 = CARTESIAN_POINT ( 'NONE',  ( 8.831537335106614961E-15, 26.23749999999999716, 12.99999999999999112 ) ) ;
#9372 = CARTESIAN_POINT ( 'NONE',  ( 19.10065816080342671, 21.75685553876272493, 5.746835883940462963 ) ) ;
#9373 = CARTESIAN_POINT ( 'NONE',  ( 17.87862548900172044, 23.19102024492039504, 6.831223922626973533 ) ) ;
#9374 = CARTESIAN_POINT ( 'NONE',  ( 18.99023649137219039, 18.99023649137212999, 4.999999999999991118 ) ) ;
#9375 = CARTESIAN_POINT ( 'NONE',  ( 0.000000000000000000, 0.000000000000000000, 20.00000000000000000 ) ) ;
#9376 = CARTESIAN_POINT ( 'NONE',  ( -10.98232076577192196, 29.09636799667091012, 1.000000000000000000 ) ) ;
#9377 = AXIS2_PLACEMENT_3D ( 'NONE', #18783, #20873, #12644 ) ;
#9378 = EDGE_CURVE ( 'NONE', #20930, #11374, #11459, .T. ) ;
#9379 = CARTESIAN_POINT ( 'NONE',  ( 18.88852612644745932, 21.54472350440676109, 12.25316411605951927 ) ) ;
#9380 = DIRECTION ( 'NONE',  ( 0.7071067811865487940, 0.7071067811865463515, 0.000000000000000000 ) ) ;
#9381 = ORIENTED_EDGE ( 'NONE', *, *, #5808, .T. ) ;
#9382 = CARTESIAN_POINT ( 'NONE',  ( 1.071796769724495668, 26.65134618820330203, 12.99999999999999112 ) ) ;
#9383 = CARTESIAN_POINT ( 'NONE',  ( 3.756430356250003655, 25.70312499938548356, 8.999999999999992895 ) ) ;
#9384 = CARTESIAN_POINT ( 'NONE',  ( 1.878215178124998497, -28.59062499938548285, 12.25316411605951927 ) ) ;
#9386 = VERTEX_POINT ( 'NONE', #13811 ) ;
#9385 = DIRECTION ( 'NONE',  ( 0.000000000000000000, 0.000000000000000000, 1.000000000000000000 ) ) ;
#9387 = CARTESIAN_POINT ( 'NONE',  ( -20.67279826512042717, 15.85973458909326084, 20.00001200000000168 ) ) ;
#9388 = CARTESIAN_POINT ( 'NONE',  ( -3.756430356250004099, -27.42812499938548143, 6.831223922626973533 ) ) ;
#9389 = VERTEX_POINT ( 'NONE', #19433 ) ;
#9390 = VERTEX_POINT ( 'NONE', #3608 ) ;
#9391 = CARTESIAN_POINT ( 'NONE',  ( 18.21624468915290507, 23.83633969896351701, 9.525109153848150711 ) ) ;
#9392 = CARTESIAN_POINT ( 'NONE',  ( 3.756430356250006319, 25.17812499938548854, 6.831223922626973533 ) ) ;
#9393 = DIRECTION ( 'NONE',  ( -0.000000000000000000, 0.000000000000000000, -1.000000000000000000 ) ) ;
#9394 = EDGE_CURVE ( 'NONE', #11934, #24237, #17149, .T. ) ;
#9395 = CARTESIAN_POINT ( 'NONE',  ( 3.999999999999997335, -27.45624999877096784, 11.30940107675849404 ) ) ;
#9396 = CARTESIAN_POINT ( 'NONE',  ( 0.000000000000000000, 0.000000000000000000, 1.000000000000000000 ) ) ;
#9397 = FACE_OUTER_BOUND ( 'NONE', #5647, .T. ) ;
#9398 = CARTESIAN_POINT ( 'NONE',  ( -2.665892461326258456, -29.88220662469441891, 11.99618178085344056 ) ) ;
#9399 = DIRECTION ( 'NONE',  ( 0.000000000000000000, 0.000000000000000000, 1.000000000000000000 ) ) ;
#9400 = CARTESIAN_POINT ( 'NONE',  ( -29.72853858738272592, 9.133673601486785643, -2.750000000000000000 ) ) ;
#9401 = CARTESIAN_POINT ( 'NONE',  ( 18.83113746560522372, 18.83113746560515622, 13.61880215351699874 ) ) ;
#9402 = B_SPLINE_CURVE_WITH_KNOTS ( 'NONE', 3,
 ( #2210, #10168, #12386, #22453, #245, #16462, #18166, #12514, #22330, #20353, #122, #18035, #8214, #2328, #16188, #4412, #18409, #11991, #20232, #10288, #6245, #14236, #20491, #22205, #19965, #6381, #18280, #368, #16072, #13977, #2587, #2448, #10551, #24034 ),
 .UNSPECIFIED., .F., .F.,
 ( 4, 2, 2, 2, 2, 2, 2, 2, 2, 2, 2, 2, 2, 2, 2, 2, 4 ),
 ( 0.000000000000000000, 0.0007824850735655043557, 0.001564970147131008711, 0.002347455220696513176, 0.003129940294262017423, 0.003912425367827521670, 0.004694910441393026351, 0.005477395514958530165, 0.006259880588524034846, 0.007042365662089539527, 0.007824850735655043341, 0.008607335809220547154, 0.009389820882786052703, 0.01017230595635155652, 0.01095479102991706033, 0.01173727610348256588, 0.01251976117704806969 ),
 .UNSPECIFIED. ) ;
#9403 = VERTEX_POINT ( 'NONE', #1791 ) ;
#9404 = CARTESIAN_POINT ( 'NONE',  ( 0.000000000000000000, 0.000000000000000000, 20.00000000000000000 ) ) ;
#9405 = DIRECTION ( 'NONE',  ( -0.000000000000000000, -0.000000000000000000, 1.000000000000000000 ) ) ;
#9406 = CARTESIAN_POINT ( 'NONE',  ( -3.756430356249996994, 25.47812499938548569, 8.999999999999992895 ) ) ;
#9408 = ADVANCED_FACE ( 'NONE', ( #9759 ), #9492, .T. ) ;
#9407 = DIRECTION ( 'NONE',  ( -0.000000000000000000, -0.000000000000000000, 1.000000000000000000 ) ) ;
#9409 = DIRECTION ( 'NONE',  ( 1.000000000000000000, 0.000000000000000000, 0.000000000000000000 ) ) ;
#9410 = CARTESIAN_POINT ( 'NONE',  ( 0.5265545572341292502, -29.99647701088549923, 12.97381592328244082 ) ) ;
#9411 = ORIENTED_EDGE ( 'NONE', *, *, #4873, .T. ) ;
#9412 = CARTESIAN_POINT ( 'NONE',  ( 1.999999999999998224, -27.04374999877096641, 12.46410161513774639 ) ) ;
#9413 = LINE ( 'NONE', #5230, #7107 ) ;
#9415 = VERTEX_POINT ( 'NONE', #23313 ) ;
#9414 = DIRECTION ( 'NONE',  ( -0.8763066800438656934, -0.4817536741017116597, 0.000000000000000000 ) ) ;
#9416 = ORIENTED_EDGE ( 'NONE', *, *, #23543, .T. ) ;
#9417 = EDGE_LOOP ( 'NONE', ( #10179, #10957, #13718, #15326 ) ) ;
#9418 = ORIENTED_EDGE ( 'NONE', *, *, #105, .T. ) ;
#9419 = ORIENTED_EDGE ( 'NONE', *, *, #5525, .T. ) ;
#9420 = CARTESIAN_POINT ( 'NONE',  ( 0.000000000000000000, 0.000000000000000000, -6.500000000000000000 ) ) ;
#9421 = CARTESIAN_POINT ( 'NONE',  ( -3.999999999999996447, -8.999999999999992895, 1.068749998770966103 ) ) ;
#9422 = CARTESIAN_POINT ( 'NONE',  ( -3.756430356249996105, 25.32812499938549067, 6.831223922626973533 ) ) ;
#9423 = CIRCLE ( 'NONE', #18208, 0.4999999999999997224 ) ;
#9424 = CARTESIAN_POINT ( 'NONE',  ( -1.878215178124995832, -5.746835883940462963, 2.990624999385481431 ) ) ;
#9425 = CARTESIAN_POINT ( 'NONE',  ( -3.999999999999996447, -8.999999999999992895, 2.868749998770965703 ) ) ;
#9426 = PRESENTATION_STYLE_ASSIGNMENT (( #3270 ) ) ;
#9427 = CARTESIAN_POINT ( 'NONE',  ( 2.672651547586948120E-15, 29.19062499938548783, 13.33755215474602984 ) ) ;
#9428 = CARTESIAN_POINT ( 'NONE',  ( 2.620986760973688460E-15, -13.61880215351699874, 3.881249998770965437 ) ) ;
#9429 = CARTESIAN_POINT ( 'NONE',  ( 3.834746474454188013E-15, 28.65624999877096712, 4.999999999999992006 ) ) ;
#9431 = ADVANCED_FACE ( 'NONE', ( #15344 ), #5023, .T. ) ;
#9430 = CARTESIAN_POINT ( 'NONE',  ( -1.999999999999995781, -5.535898384862237620, 1.500000000000001332 ) ) ;
#9432 = CARTESIAN_POINT ( 'NONE',  ( 3.469446951953614189E-15, 30.00000000000000355, 8.999999999999992895 ) ) ;
#9433 = DIRECTION ( 'NONE',  ( 1.000000000000000000, 0.000000000000000000, 0.000000000000000000 ) ) ;
#9434 = CARTESIAN_POINT ( 'NONE',  ( -4.000000000000001776, -29.46250000000000213, 11.30940107675849760 ) ) ;
#9435 = CARTESIAN_POINT ( 'NONE',  ( 1.999999999999998224, -27.04374999877096641, 12.46410161513774639 ) ) ;
#9436 = CARTESIAN_POINT ( 'NONE',  ( 1.878215178125000939, -12.25316411605952283, 4.228124999385483918 ) ) ;
#9437 = DIRECTION ( 'NONE',  ( 0.000000000000000000, 0.000000000000000000, 1.000000000000000000 ) ) ;
#9438 = CARTESIAN_POINT ( 'NONE',  ( -3.999999999999996447, -8.999999999999992895, 3.318749998770968102 ) ) ;
#9439 = CARTESIAN_POINT ( 'NONE',  ( -4.000000000000001776, -25.86250000000000071, 11.30940107675849760 ) ) ;
#9440 = EDGE_LOOP ( 'NONE', ( #25803, #19374, #22919, #21486 ) ) ;
#9441 = DIRECTION ( 'NONE',  ( 0.000000000000000000, 0.000000000000000000, 1.000000000000000000 ) ) ;
#9442 = ORIENTED_EDGE ( 'NONE', *, *, #9343, .F. ) ;
#9443 = EDGE_CURVE ( 'NONE', #51, #23094, #8793, .T. ) ;
#9444 = ORIENTED_EDGE ( 'NONE', *, *, #20059, .F. ) ;
#9445 = CYLINDRICAL_SURFACE ( 'NONE', #14977, 24.00000000000000355 ) ;
#9446 = VERTEX_POINT ( 'NONE', #3446 ) ;
#9447 = CARTESIAN_POINT ( 'NONE',  ( -3.756430356250002323, -28.36562499938548854, 11.16877607737301226 ) ) ;
#9448 = ORIENTED_EDGE ( 'NONE', *, *, #20801, .F. ) ;
#9449 = CARTESIAN_POINT ( 'NONE',  ( 2.000000000000003997, 26.87500000000000355, 5.535898384862238508 ) ) ;
#9450 = EDGE_LOOP ( 'NONE', ( #11879, #24235, #9830, #1952 ) ) ;
#9451 = CARTESIAN_POINT ( 'NONE',  ( -1.999999999999995781, 28.30000000000000071, 5.535898384862237620 ) ) ;
#9452 = DIRECTION ( 'NONE',  ( 0.000000000000000000, 0.000000000000000000, -1.000000000000000000 ) ) ;
#9453 = CARTESIAN_POINT ( 'NONE',  ( -3.918623196469520842, 31.50000000000000000, 4.456389954662587805 ) ) ;
#9454 = CARTESIAN_POINT ( 'NONE',  ( 0.000000000000000000, 0.000000000000000000, 15.00000000000000178 ) ) ;
#9455 = CARTESIAN_POINT ( 'NONE',  ( 22.76675617620853131, 17.45436142028971460, 6.831223922626973533 ) ) ;
#9456 =( BOUNDED_CURVE ( )  B_SPLINE_CURVE ( 2, ( #12946, #3010, #10979, #21175, #25867, #25351, #7954, #25737, #3519 ),
 .UNSPECIFIED., .F., .F. ) 
 B_SPLINE_CURVE_WITH_KNOTS ( ( 3, 2, 2, 2, 3 ),
 ( 0.9250000000000000444, 0.9333333333333333481, 0.9499999999999999556, 0.9666666666666666741, 0.9749999999999999778 ),
 .UNSPECIFIED. ) 
 CURVE ( )  GEOMETRIC_REPRESENTATION_ITEM ( )  RATIONAL_B_SPLINE_CURVE ( ( 0.9330127018922194093, 0.9330127018922198534, 1.000000000000000000, 0.8660254037844387076, 1.000000000000000000, 0.8660254037844387076, 1.000000000000000000, 0.9330127018922194093, 0.9330127018922194093 ) ) 
 REPRESENTATION_ITEM ( '' )  );
#9457 = CARTESIAN_POINT ( 'NONE',  ( -3.756430356250003655, -25.25312499938548427, 8.999999999999992895 ) ) ;
#9458 = EDGE_CURVE ( 'NONE', #14350, #12673, #4888, .T. ) ;
#9459 = CARTESIAN_POINT ( 'NONE',  ( 3.752267015613588906E-15, 26.91250000000000142, 4.381197846482986158 ) ) ;
#9460 = EDGE_CURVE ( 'NONE', #2153, #22574, #16315, .T. ) ;
#9461 = CARTESIAN_POINT ( 'NONE',  ( 17.69528343319515784, 20.35148081115446317, 12.25316411605951927 ) ) ;
#9462 = CARTESIAN_POINT ( 'NONE',  ( 2.000000000000003997, 26.81874999877096855, 5.535898384862238508 ) ) ;
#9463 = ORIENTED_EDGE ( 'NONE', *, *, #15852, .T. ) ;
#9465 = EDGE_CURVE ( 'NONE', #16189, #22108, #15273, .T. ) ;
#9464 = VERTEX_POINT ( 'NONE', #22813 ) ;
#9466 = CARTESIAN_POINT ( 'NONE',  ( 6.009258394948636914E-15, 27.30624999877097636, 4.381197846482986158 ) ) ;
#9467 = CYLINDRICAL_SURFACE ( 'NONE', #21665, 4.000000000000000000 ) ;
#9468 = ORIENTED_EDGE ( 'NONE', *, *, #9005, .T. ) ;
#9469 = CARTESIAN_POINT ( 'NONE',  ( 4.000000000000001776, 29.85624999877096997, 11.30940107675849760 ) ) ;
#9470 = CARTESIAN_POINT ( 'NONE',  ( 3.756430356250002323, 28.81562499938548427, 11.16877607737301226 ) ) ;
#9471 = ADVANCED_FACE ( 'NONE', ( #7367 ), #18890, .T. ) ;
#9472 = ORIENTED_EDGE ( 'NONE', *, *, #12593, .T. ) ;
#9473 = ORIENTED_EDGE ( 'NONE', *, *, #16940, .F. ) ;
#9474 = CARTESIAN_POINT ( 'NONE',  ( -3.999999999999996447, -8.999999999999992895, 4.275000000000001243 ) ) ;
#9475 = ORIENTED_EDGE ( 'NONE', *, *, #15387, .T. ) ;
#9476 = CARTESIAN_POINT ( 'NONE',  ( 3.756430356249996105, -28.14062499938548356, 6.831223922626973533 ) ) ;
#9477 = CARTESIAN_POINT ( 'NONE',  ( 3.735045420075836212E-15, 25.70312499938548001, 4.662447845253954171 ) ) ;
#9478 = CARTESIAN_POINT ( 'NONE',  ( -3.756430356249996549, 27.65312499938548996, 11.16877607737301048 ) ) ;
#9479 = CARTESIAN_POINT ( 'NONE',  ( 0.000000000000000000, 0.000000000000000000, -6.500000000000000000 ) ) ;
#9480 = CARTESIAN_POINT ( 'NONE',  ( -3.999999999999998224, 27.02500000000000213, 8.999999999999992895 ) ) ;
#9481 = CARTESIAN_POINT ( 'NONE',  ( 3.756430356250002323, 27.35312499938547859, 11.16877607737301226 ) ) ;
#9482 = CARTESIAN_POINT ( 'NONE',  ( -14.98253926456298579, 27.25313774936435962, 1.000000000000000000 ) ) ;
#9483 = CARTESIAN_POINT ( 'NONE',  ( 0.000000000000000000, 0.000000000000000000, -6.500000000000000000 ) ) ;
#9484 = CARTESIAN_POINT ( 'NONE',  ( -1.878215178124995832, 25.74062499938548498, 5.746835883940462963 ) ) ;
#9485 = CARTESIAN_POINT ( 'NONE',  ( -1.071796769724490783, 27.06115380933863790, 12.99999999999999289 ) ) ;
#9486 = CARTESIAN_POINT ( 'NONE',  ( 21.43417430471724927, 15.77732005522480563, 11.30940107675849760 ) ) ;
#9487 = CARTESIAN_POINT ( 'NONE',  ( 22.39552511608559371, 17.08313036016677700, 11.16877607737301226 ) ) ;
#9488 = CARTESIAN_POINT ( 'NONE',  ( 0.000000000000000000, 0.000000000000000000, 16.00000000000000000 ) ) ;
#9489 = CARTESIAN_POINT ( 'NONE',  ( 0.000000000000000000, 10.00000000000000000, 15.00000000000000178 ) ) ;
#9490 = FACE_OUTER_BOUND ( 'NONE', #21981, .T. ) ;
#9491 = CARTESIAN_POINT ( 'NONE',  ( 22.02429405596265610, 16.71189930004383584, 8.999999999999992895 ) ) ;
#9492 = PLANE ( 'NONE',  #9203 ) ;
#9493 = VERTEX_POINT ( 'NONE', #9457 ) ;
#9494 = CARTESIAN_POINT ( 'NONE',  ( 8.831537335106614961E-15, 26.63124999877096855, 12.99999999999999112 ) ) ;
#9495 = CARTESIAN_POINT ( 'NONE',  ( 3.999999999999996003, -25.63749999999999929, 6.690598923241487306 ) ) ;
#9496 = ADVANCED_FACE ( 'NONE', ( #15225 ), #13004, .F. ) ;
#9498 = ORIENTED_EDGE ( 'NONE', *, *, #16501, .T. ) ;
#9497 = DIRECTION ( 'NONE',  ( 1.000000000000000000, 0.000000000000000000, 0.000000000000000000 ) ) ;
#9499 = CARTESIAN_POINT ( 'NONE',  ( 3.756430356250003655, 27.05312499938548498, 8.999999999999992895 ) ) ;
#9500 = EDGE_CURVE ( 'NONE', #485, #1055, #21223, .T. ) ;
#9501 = CARTESIAN_POINT ( 'NONE',  ( 1.071796769724488563, -29.76115380933863364, 12.99999999999999289 ) ) ;
#9502 = CARTESIAN_POINT ( 'NONE',  ( -1.701696020694479783, 25.99999999999999645, 20.00001200000000523 ) ) ;
#9503 = CARTESIAN_POINT ( 'NONE',  ( 1.878215178124998497, -27.24062499938548498, 12.25316411605951927 ) ) ;
#9504 = ORIENTED_EDGE ( 'NONE', *, *, #13555, .F. ) ;
#9505 = VERTEX_POINT ( 'NONE', #7246 ) ;
#9506 = CARTESIAN_POINT ( 'NONE',  ( 3.110308778861350376, 34.50000000000000000, 14.13088484572963033 ) ) ;
#9507 = CARTESIAN_POINT ( 'NONE',  ( 3.756430356250002323, 25.62812499938548072, 6.831223922626973533 ) ) ;
#9508 = CARTESIAN_POINT ( 'NONE',  ( 3.735045420075836212E-15, -4.662447845253954171, 0.7031249993854805647 ) ) ;
#9509 = CIRCLE ( 'NONE', #25382, 0.5000000000000013323 ) ;
#9510 = CARTESIAN_POINT ( 'NONE',  ( 3.756430356250004099, -6.831223922626973533, 3.440624999385483829 ) ) ;
#9511 = DIRECTION ( 'NONE',  ( 1.000000000000000000, 0.000000000000000000, 0.000000000000000000 ) ) ;
#9512 = DIRECTION ( 'NONE',  ( 1.000000000000000000, 0.000000000000000000, 0.000000000000000000 ) ) ;
#9513 = LINE ( 'NONE', #23008, #2551 ) ;
#9514 = AXIS2_PLACEMENT_3D ( 'NONE', #16606, #20259, #4834 ) ;
#9515 = DIRECTION ( 'NONE',  ( 0.000000000000000000, 0.000000000000000000, 1.000000000000000000 ) ) ;
#9516 = CARTESIAN_POINT ( 'NONE',  ( 27.25313774936409317, -14.98253926456347074, 1.000000000000000000 ) ) ;
#9517 = DIRECTION ( 'NONE',  ( -0.000000000000000000, -0.000000000000000000, 1.000000000000000000 ) ) ;
#9518 = CARTESIAN_POINT ( 'NONE',  ( 17.07220934740368889, 19.90063647214981302, 12.46410161513774639 ) ) ;
#9519 = ORIENTED_EDGE ( 'NONE', *, *, #8233, .F. ) ;
#9520 = DIRECTION ( 'NONE',  ( -0.000000000000000000, -0.000000000000000000, -1.000000000000000000 ) ) ;
#9521 = CARTESIAN_POINT ( 'NONE',  ( -3.756430356250002323, -28.81562499938548427, 11.16877607737301226 ) ) ;
#9522 = CARTESIAN_POINT ( 'NONE',  ( -3.756430356249996994, 26.82812499938548711, 8.999999999999992895 ) ) ;
#9523 = CARTESIAN_POINT ( 'NONE',  ( 3.834746474454188013E-15, 28.26249999999999929, 4.999999999999992006 ) ) ;
#9524 = DIRECTION ( 'NONE',  ( 0.000000000000000000, -0.000000000000000000, 1.000000000000000000 ) ) ;
#9525 = EDGE_CURVE ( 'NONE', #18011, #7791, #5276, .T. ) ;
#9526 = CARTESIAN_POINT ( 'NONE',  ( -1.057460391440397258E-14, 29.10624999877096641, 4.999999999999992006 ) ) ;
#9527 = VERTEX_POINT ( 'NONE', #23074 ) ;
#9528 = DIRECTION ( 'NONE',  ( -0.000000000000000000, -1.000000000000000000, -0.000000000000000000 ) ) ;
#9529 = CARTESIAN_POINT ( 'NONE',  ( 3.756430356249995661, -25.32812499938548356, 6.831223922626973533 ) ) ;
#9531 = ORIENTED_EDGE ( 'NONE', *, *, #14503, .F. ) ;
#9530 = CARTESIAN_POINT ( 'NONE',  ( -10.98232076577242466, -29.09636799667071116, -6.500000000000000000 ) ) ;
#9532 = ADVANCED_FACE ( 'NONE', ( #15100 ), #11031, .T. ) ;
#9533 = EDGE_LOOP ( 'NONE', ( #23783, #24370, #11015, #6513 ) ) ;
#9534 = AXIS2_PLACEMENT_3D ( 'NONE', #18448, #24456, #6534 ) ;
#9535 = ORIENTED_EDGE ( 'NONE', *, *, #18400, .F. ) ;
#9536 = EDGE_LOOP ( 'NONE', ( #16438, #23920, #14697, #9531 ) ) ;
#9537 = ORIENTED_EDGE ( 'NONE', *, *, #18300, .F. ) ;
#9538 = DIRECTION ( 'NONE',  ( 0.000000000000000000, 0.000000000000000000, 1.000000000000000000 ) ) ;
#9539 = CARTESIAN_POINT ( 'NONE',  ( 28.14012133169314822, -13.24173596767388794, 1.000000000000000000 ) ) ;
#9540 = AXIS2_PLACEMENT_3D ( 'NONE', #15202, #19367, #5133 ) ;
#9541 = ADVANCED_FACE ( 'NONE', ( #1094 ), #9069, .T. ) ;
#9542 = CARTESIAN_POINT ( 'NONE',  ( -22.67092431280563503, 21.28941499438250062, 1.000000000000000000 ) ) ;
#9543 = CARTESIAN_POINT ( 'NONE',  ( 3.756430356250004099, -6.831223922626973533, 2.428124999385481431 ) ) ;
#9544 = CARTESIAN_POINT ( 'NONE',  ( 4.000000000000003553, -6.690598923241489970, 2.231249998770966858 ) ) ;
#9545 = CARTESIAN_POINT ( 'NONE',  ( -1.878215178124998497, 27.80312499938548498, 12.25316411605951927 ) ) ;
#9546 = CARTESIAN_POINT ( 'NONE',  ( 3.999999999999987121, -11.30940107675850648, 3.956249998770966947 ) ) ;
#9547 = AXIS2_PLACEMENT_3D ( 'NONE', #23019, #7315, #24968 ) ;
#9548 = CARTESIAN_POINT ( 'NONE',  ( 20.89942480057588980, 20.89942480057579033, 4.999999999999992006 ) ) ;
#9549 = CARTESIAN_POINT ( 'NONE',  ( -1.999999999999995781, -5.535898384862237620, 1.950000000000000400 ) ) ;
#9550 = CARTESIAN_POINT ( 'NONE',  ( 0.000000000000000000, 0.000000000000000000, -6.500000000000000000 ) ) ;
#9551 = FACE_OUTER_BOUND ( 'NONE', #162, .T. ) ;
#9552 = CARTESIAN_POINT ( 'NONE',  ( 4.000000000000003553, 25.19687499938548569, 8.999999999999992895 ) ) ;
#9553 = CARTESIAN_POINT ( 'NONE',  ( 1.999999999999995781, -25.99374999877096926, 5.535898384862237620 ) ) ;
#9554 = CARTESIAN_POINT ( 'NONE',  ( 1.878215178125004048, 27.12812499938548783, 5.746835883940462963 ) ) ;
#9555 = AXIS2_PLACEMENT_3D ( 'NONE', #11949, #2404, #10508 ) ;
#9556 = FACE_BOUND ( 'NONE', #14922, .T. ) ;
#9558 = CIRCLE ( 'NONE', #14158, 31.10000000000000142 ) ;
#9557 = CARTESIAN_POINT ( 'NONE',  ( 2.000000000000000888, -12.46410161513774817, 4.818749998770965881 ) ) ;
#9559 = FACE_OUTER_BOUND ( 'NONE', #24729, .T. ) ;
#9560 = ORIENTED_EDGE ( 'NONE', *, *, #17459, .T. ) ;
#9561 = CARTESIAN_POINT ( 'NONE',  ( 1.500000000000001776, -10.49999999999999289, 25.00000000000000000 ) ) ;
#9562 = ORIENTED_EDGE ( 'NONE', *, *, #23054, .T. ) ;
#9563 = EDGE_CURVE ( 'NONE', #15156, #20673, #11282, .T. ) ;
#9564 = ORIENTED_EDGE ( 'NONE', *, *, #11490, .F. ) ;
#9565 = CARTESIAN_POINT ( 'NONE',  ( -0.7500000000000000000, -1.299038105676658450, 17.69999999999999929 ) ) ;
#9566 = EDGE_LOOP ( 'NONE', ( #8343, #11080, #5736, #16083 ) ) ;
#9567 = CARTESIAN_POINT ( 'NONE',  ( 3.756430356249995661, -29.04062499938548569, 6.831223922626973533 ) ) ;
#9568 = ORIENTED_EDGE ( 'NONE', *, *, #11117, .F. ) ;
#9569 = DIRECTION ( 'NONE',  ( 0.5358267949790093132, 0.8443279255020070817, 0.000000000000000000 ) ) ;
#9570 = EDGE_CURVE ( 'NONE', #5581, #14528, #20053, .T. ) ;
#9571 = VECTOR ( 'NONE', #25832, 1000.000000000000000 ) ;
#9572 = ORIENTED_EDGE ( 'NONE', *, *, #23291, .F. ) ;
#9573 = CARTESIAN_POINT ( 'NONE',  ( -3.999999999999997335, 26.61250000000000071, 11.30940107675849404 ) ) ;
#9574 = CARTESIAN_POINT ( 'NONE',  ( -30.53863125411927371, -1.952785157361310198, -6.500000000000000000 ) ) ;
#9575 = VECTOR ( 'NONE', #3566, 1000.000000000000000 ) ;
#9576 = EDGE_CURVE ( 'NONE', #1614, #10560, #20935, .T. ) ;
#9577 = VECTOR ( 'NONE', #5106, 1000.000000000000000 ) ;
#9578 = CARTESIAN_POINT ( 'NONE',  ( -30.12293631110050995, -7.734255490826679846, -6.500000000000000000 ) ) ;
#9579 = DIRECTION ( 'NONE',  ( -0.5877852522924652545, 0.8090169943749532244, 0.000000000000000000 ) ) ;
#9580 = CARTESIAN_POINT ( 'NONE',  ( 23.37663577498192780, 18.06424101906310753, 8.999999999999992895 ) ) ;
#9581 = CARTESIAN_POINT ( 'NONE',  ( 0.000000000000000000, 0.000000000000000000, -6.500000000000000000 ) ) ;
#9582 = AXIS2_PLACEMENT_3D ( 'NONE', #8250, #14014, #15984 ) ;
#9583 = CARTESIAN_POINT ( 'NONE',  ( 2.620986760973688460E-15, 27.13750000000000284, 13.61880215351699874 ) ) ;
#9584 = VECTOR ( 'NONE', #23221, 1000.000000000000000 ) ;
#9585 = CARTESIAN_POINT ( 'NONE',  ( 18.86200962215296784, 21.51820700011226606, 5.746835883940462963 ) ) ;
#9586 = CARTESIAN_POINT ( 'NONE',  ( -2.000000000000003997, -29.51874999877096784, 5.535898384862238508 ) ) ;
#9587 = CIRCLE ( 'NONE', #25456, 0.5000000000000017764 ) ;
#9588 = VERTEX_POINT ( 'NONE', #2130 ) ;
#9589 = ORIENTED_EDGE ( 'NONE', *, *, #22140, .T. ) ;
#9590 = CARTESIAN_POINT ( 'NONE',  ( -1.999999999999994893, 29.14374999877097139, 5.535898384862237620 ) ) ;
#9591 = CIRCLE ( 'NONE', #12944, 0.4999999999999999445 ) ;
#9592 = ORIENTED_EDGE ( 'NONE', *, *, #6160, .T. ) ;
#9593 = AXIS2_PLACEMENT_3D ( 'NONE', #7917, #23618, #1650 ) ;
#9594 = CARTESIAN_POINT ( 'NONE',  ( -3.756430356249995661, 27.24062499938548498, 6.831223922626973533 ) ) ;
#9595 = CARTESIAN_POINT ( 'NONE',  ( -1.999999999999995781, 27.34374999877097068, 5.535898384862237620 ) ) ;
#9596 = ORIENTED_EDGE ( 'NONE', *, *, #13690, .F. ) ;
#9597 = ORIENTED_EDGE ( 'NONE', *, *, #13421, .F. ) ;
#9598 =( BOUNDED_CURVE ( )  B_SPLINE_CURVE ( 2, ( #20978, #25017, #16658, #7106, #15220, #14706, #6975, #2925, #10632 ),
 .UNSPECIFIED., .F., .F. ) 
 B_SPLINE_CURVE_WITH_KNOTS ( ( 3, 2, 2, 2, 3 ),
 ( 0.3750000000000000000, 0.3833333333333333592, 0.4000000000000000222, 0.4166666666666666852, 0.4250000000000000444 ),
 .UNSPECIFIED. ) 
 CURVE ( )  GEOMETRIC_REPRESENTATION_ITEM ( )  RATIONAL_B_SPLINE_CURVE ( ( 0.9330127018922194093, 0.9330127018922194093, 1.000000000000000000, 0.8660254037844387076, 1.000000000000000000, 0.8660254037844387076, 1.000000000000000000, 0.9330127018922191873, 0.9330127018922194093 ) ) 
 REPRESENTATION_ITEM ( '' )  );
#9599 = EDGE_CURVE ( 'NONE', #7412, #486, #2734, .T. ) ;
#9600 = FACE_OUTER_BOUND ( 'NONE', #826, .T. ) ;
#9601 = AXIS2_PLACEMENT_3D ( 'NONE', #13850, #4031, #14106 ) ;
#9602 = ORIENTED_EDGE ( 'NONE', *, *, #15921, .F. ) ;
#9603 = CARTESIAN_POINT ( 'NONE',  ( -25.98730014090425300, 17.08421000182794813, 1.000000000000000000 ) ) ;
#9604 = DIRECTION ( 'NONE',  ( -1.000000000000000000, 0.000000000000000000, 0.000000000000000000 ) ) ;
#9605 =( BOUNDED_CURVE ( )  B_SPLINE_CURVE ( 2, ( #15564, #19469, #11497, #19850, #3525, #7962, #23655, #17513, #17775 ),
 .UNSPECIFIED., .F., .T. ) 
 B_SPLINE_CURVE_WITH_KNOTS ( ( 3, 2, 2, 2, 3 ),
 ( 0.2750000000000000222, 0.2833333333333333259, 0.2999999999999999889, 0.3166666666666666519, 0.3250000000000000111 ),
 .UNSPECIFIED. ) 
 CURVE ( )  GEOMETRIC_REPRESENTATION_ITEM ( )  RATIONAL_B_SPLINE_CURVE ( ( 0.9330127018922194093, 0.9330127018922196314, 1.000000000000000000, 0.8660254037844387076, 1.000000000000000000, 0.8660254037844387076, 1.000000000000000000, 0.9330127018922191873, 0.9330127018922194093 ) ) 
 REPRESENTATION_ITEM ( '' )  );
#9606 = CARTESIAN_POINT ( 'NONE',  ( 3.756430356250006319, 28.77812499938548640, 6.831223922626973533 ) ) ;
#9607 = AXIS2_PLACEMENT_3D ( 'NONE', #9170, #17160, #23169 ) ;
#9608 = EDGE_CURVE ( 'NONE', #21413, #10718, #3787, .T. ) ;
#9609 = ADVANCED_FACE ( 'NONE', ( #23580 ), #5661, .T. ) ;
#9610 = FACE_OUTER_BOUND ( 'NONE', #22921, .T. ) ;
#9611 = CARTESIAN_POINT ( 'NONE',  ( -3.999999999999999556, 26.61250000000000426, 11.30940107675849404 ) ) ;
#9612 = AXIS2_PLACEMENT_3D ( 'NONE', #24087, #297, #13907 ) ;
#9613 = EDGE_CURVE ( 'NONE', #11934, #19625, #12147, .T. ) ;
#9614 = CARTESIAN_POINT ( 'NONE',  ( -3.756430356249995661, 28.92812499938548143, 6.831223922626973533 ) ) ;
#9615 = DIRECTION ( 'NONE',  ( 0.8763066800438685799, 0.4817536741017063306, 0.000000000000000000 ) ) ;
#9616 = CARTESIAN_POINT ( 'NONE',  ( 1.999999999999995781, -28.69374999877096855, 5.535898384862237620 ) ) ;
#9617 = CARTESIAN_POINT ( 'NONE',  ( 1.071796769724492338, 28.95759618943233704, 12.99999999999999467 ) ) ;
#9618 = VECTOR ( 'NONE', #24407, 1000.000000000000000 ) ;
#9619 = CARTESIAN_POINT ( 'NONE',  ( -4.000000000000003553, -29.73213749463701561, 8.999999999999992895 ) ) ;
#9620 = CARTESIAN_POINT ( 'NONE',  ( 18.87091222291602222, 18.87091222291595827, 13.61880215351699874 ) ) ;
#9621 = CARTESIAN_POINT ( 'NONE',  ( 16.95054783869437642, 22.26294259461305103, 8.999999999999992895 ) ) ;
#9622 = CARTESIAN_POINT ( 'NONE',  ( 30.91344420362548107, 3.401318489840985837, -2.750000000000000000 ) ) ;
#9623 = CARTESIAN_POINT ( 'NONE',  ( 1.878215178125004048, 29.26562499938548356, 5.746835883940462963 ) ) ;
#9624 = CIRCLE ( 'NONE', #24244, 0.5000000000000005551 ) ;
#9625 = LINE ( 'NONE', #3349, #14167 ) ;
#9626 = AXIS2_PLACEMENT_3D ( 'NONE', #1485, #19393, #21104 ) ;
#9627 = DIRECTION ( 'NONE',  ( 0.000000000000000000, 0.000000000000000000, 1.000000000000000000 ) ) ;
#9628 = CARTESIAN_POINT ( 'NONE',  ( 2.000000000000003553, 25.91874999877097352, 5.535898384862238508 ) ) ;
#9629 = ORIENTED_EDGE ( 'NONE', *, *, #6132, .T. ) ;
#9630 = CARTESIAN_POINT ( 'NONE',  ( -3.999999999999997335, 26.10624999877096997, 11.30940107675849404 ) ) ;
#9631 = ADVANCED_FACE ( 'NONE', ( #10094 ), #1752, .T. ) ;
#9632 = CARTESIAN_POINT ( 'NONE',  ( 1.999999999999995781, -25.60000000000000142, 5.535898384862237620 ) ) ;
#9634 = ORIENTED_EDGE ( 'NONE', *, *, #20217, .T. ) ;
#9633 = CARTESIAN_POINT ( 'NONE',  ( 2.003086131649545506E-15, 25.59062499938548996, 13.33755215474603162 ) ) ;
#9635 = CARTESIAN_POINT ( 'NONE',  ( 3.735045420075836212E-15, 27.61562499938548498, 4.662447845253954171 ) ) ;
#9636 = VECTOR ( 'NONE', #10157, 1000.000000000000000 ) ;
#9637 = FACE_OUTER_BOUND ( 'NONE', #11912, .T. ) ;
#9638 = CARTESIAN_POINT ( 'NONE',  ( 22.56362157461193618, 13.02991752792604174, 20.00001200000000168 ) ) ;
#9639 = CARTESIAN_POINT ( 'NONE',  ( 0.000000000000000000, 0.000000000000000000, 19.59999999999999787 ) ) ;
#9640 = ORIENTED_EDGE ( 'NONE', *, *, #4807, .T. ) ;
#9641 = ORIENTED_EDGE ( 'NONE', *, *, #707, .T. ) ;
#9642 = CARTESIAN_POINT ( 'NONE',  ( -3.756430356249996105, 25.40312499938548640, 11.16877607737301226 ) ) ;
#9643 = CARTESIAN_POINT ( 'NONE',  ( 3.756430356250003655, -8.999999999999992895, 0.5906249993854819635 ) ) ;
#9644 = ADVANCED_FACE ( 'NONE', ( #9721 ), #17568, .T. ) ;
#9645 = AXIS2_PLACEMENT_3D ( 'NONE', #24878, #7220, #24607 ) ;
#9646 = AXIS2_PLACEMENT_3D ( 'NONE', #18823, #16603, #16487 ) ;
#9647 = FACE_OUTER_BOUND ( 'NONE', #13261, .T. ) ;
#9648 = SURFACE_STYLE_FILL_AREA ( #23248 ) ;
#9649 = EDGE_CURVE ( 'NONE', #16676, #18810, #25519, .T. ) ;
#9650 = CARTESIAN_POINT ( 'NONE',  ( -2.000000000000003997, -27.32500000000000284, 5.535898384862238508 ) ) ;
#9652 = ADVANCED_FACE ( 'NONE', ( #11925 ), #23831, .T. ) ;
#9651 = VECTOR ( 'NONE', #3094, 1000.000000000000000 ) ;
#9653 = CARTESIAN_POINT ( 'NONE',  ( 2.000000000000000000, 28.97500000000000853, 12.46410161513774817 ) ) ;
#9654 = CARTESIAN_POINT ( 'NONE',  ( -30.54913349766228592, -5.827558883615738594, -6.500000000000000000 ) ) ;
#9655 = LINE ( 'NONE', #9275, #17451 ) ;
#9656 = DIRECTION ( 'NONE',  ( -0.9980267284282710039, 0.06279051952932233893, 0.000000000000000000 ) ) ;
#9657 = CARTESIAN_POINT ( 'NONE',  ( 15.30652457243565223, 20.61891932835433394, 11.16877607737301226 ) ) ;
#9658 = CYLINDRICAL_SURFACE ( 'NONE', #9713, 0.5000000000000004441 ) ;
#9659 = VERTEX_POINT ( 'NONE', #23698 ) ;
#9660 = DIRECTION ( 'NONE',  ( -0.4257792915650642218, 0.9048270524660235736, 0.000000000000000000 ) ) ;
#9661 = CARTESIAN_POINT ( 'NONE',  ( 11.91206721063051432, 28.72825533807128551, -2.750000000000000000 ) ) ;
#9662 = CARTESIAN_POINT ( 'NONE',  ( 1.878215178125004048, 27.12812499938548783, 5.746835883940462963 ) ) ;
#9663 = CARTESIAN_POINT ( 'NONE',  ( 3.752267015613588906E-15, -4.381197846482986158, 2.362499999999997602 ) ) ;
#9664 = AXIS2_PLACEMENT_3D ( 'NONE', #22685, #4770, #16541 ) ;
#9665 = CARTESIAN_POINT ( 'NONE',  ( -3.999999999999996447, 26.51874999877097139, 8.999999999999992895 ) ) ;
#9666 = DIRECTION ( 'NONE',  ( 0.000000000000000000, 1.000000000000000000, 0.000000000000000000 ) ) ;
#9667 = ORIENTED_EDGE ( 'NONE', *, *, #10121, .F. ) ;
#9668 = CARTESIAN_POINT ( 'NONE',  ( -9.133673601486059113, 29.72853858738294619, -6.500000000000000000 ) ) ;
#9669 = CARTESIAN_POINT ( 'NONE',  ( -1.952785157361201618, 31.03863125411927371, -6.500000000000000000 ) ) ;
#9671 = EDGE_LOOP ( 'NONE', ( #16472, #10261, #6838, #25013 ) ) ;
#9670 = CARTESIAN_POINT ( 'NONE',  ( 0.000000000000000000, 0.000000000000000000, 19.00000000000000000 ) ) ;
#9672 = CIRCLE ( 'NONE', #10905, 31.10000000000000142 ) ;
#9673 = VERTEX_POINT ( 'NONE', #9963 ) ;
#9674 = VERTEX_POINT ( 'NONE', #3571 ) ;
#9675 = EDGE_LOOP ( 'NONE', ( #6704, #14321, #19847, #8875 ) ) ;
#9676 = ORIENTED_EDGE ( 'NONE', *, *, #15880, .T. ) ;
#9677 = DIRECTION ( 'NONE',  ( 0.1873813145857189666, -0.9822872507286897203, 0.000000000000000000 ) ) ;
#9679 = DIRECTION ( 'NONE',  ( -0.000000000000000000, 0.000000000000000000, -1.000000000000000000 ) ) ;
#9678 = AXIS2_PLACEMENT_3D ( 'NONE', #21680, #7697, #5723 ) ;
#9680 = FACE_OUTER_BOUND ( 'NONE', #23184, .T. ) ;
#9681 = CARTESIAN_POINT ( 'NONE',  ( -3.999999999999994671, 27.88750000000000639, 6.690598923241487306 ) ) ;
#9682 = AXIS2_PLACEMENT_3D ( 'NONE', #4003, #25842, #21922 ) ;
#9683 = CARTESIAN_POINT ( 'NONE',  ( -1.878215178124998497, -12.25316411605951927, 3.140624999385482230 ) ) ;
#9684 = CARTESIAN_POINT ( 'NONE',  ( 2.000000000000000888, -12.46410161513774817, 2.118749998770968368 ) ) ;
#9685 = ADVANCED_FACE ( 'NONE', ( #5778 ), #17954, .F. ) ;
#9686 = AXIS2_PLACEMENT_3D ( 'NONE', #25130, #3659, #1714 ) ;
#9687 = CARTESIAN_POINT ( 'NONE',  ( 3.756430356250002323, 29.26562499938548356, 11.16877607737301226 ) ) ;
#9688 = ADVANCED_FACE ( 'NONE', ( #6048 ), #13524, .T. ) ;
#9689 = CARTESIAN_POINT ( 'NONE',  ( 8.831537335106614961E-15, 27.53124999877097068, 12.99999999999999112 ) ) ;
#9690 = DIRECTION ( 'NONE',  ( -0.7071067811865487940, -0.7071067811865463515, 0.000000000000000000 ) ) ;
#9691 = CARTESIAN_POINT ( 'NONE',  ( -3.999999999999996003, -6.690598923241487306, 1.537500000000000089 ) ) ;
#9692 = CARTESIAN_POINT ( 'NONE',  ( 0.000000000000000000, 0.000000000000000000, 1.000000000000000000 ) ) ;
#9693 = CARTESIAN_POINT ( 'NONE',  ( 20.62100150635272300, 20.62100150635266260, 4.999999999999992006 ) ) ;
#9694 = DIRECTION ( 'NONE',  ( 0.8660254037844397068, -0.4999999999999983347, 0.000000000000000000 ) ) ;
#9695 = CARTESIAN_POINT ( 'NONE',  ( 3.999999999999997335, -25.65624999877097068, 11.30940107675849404 ) ) ;
#9696 = EDGE_CURVE ( 'NONE', #16624, #3323, #5877, .T. ) ;
#9697 = AXIS2_PLACEMENT_3D ( 'NONE', #11988, #2325, #13974 ) ;
#9698 = CARTESIAN_POINT ( 'NONE',  ( 3.756430356250002323, 27.46562499938548640, 11.16877607737301226 ) ) ;
#9699 = DIRECTION ( 'NONE',  ( 0.000000000000000000, 0.000000000000000000, 1.000000000000000000 ) ) ;
#9700 = CARTESIAN_POINT ( 'NONE',  ( 1.859271017917182139E-15, 29.78124999877096712, 12.99999999999999289 ) ) ;
#9701 = CYLINDRICAL_SURFACE ( 'NONE', #2209, 4.000000000000000000 ) ;
#9702 = ORIENTED_EDGE ( 'NONE', *, *, #17934, .F. ) ;
#9703 = CARTESIAN_POINT ( 'NONE',  ( -1.057460391440397258E-14, 28.71250000000000213, 4.999999999999992006 ) ) ;
#9704 = ORIENTED_EDGE ( 'NONE', *, *, #13690, .T. ) ;
#9705 = AXIS2_PLACEMENT_3D ( 'NONE', #6296, #12037, #2374 ) ;
#9706 = ORIENTED_EDGE ( 'NONE', *, *, #19420, .T. ) ;
#9707 = DIRECTION ( 'NONE',  ( -0.000000000000000000, -1.000000000000000000, -0.000000000000000000 ) ) ;
#9708 = ORIENTED_EDGE ( 'NONE', *, *, #25661, .F. ) ;
#9709 = CARTESIAN_POINT ( 'NONE',  ( 3.756430356249997882, -26.86562499938548498, 11.16877607737301226 ) ) ;
#9710 = EDGE_LOOP ( 'NONE', ( #18082, #6992, #17551, #15727 ) ) ;
#9711 = DIRECTION ( 'NONE',  ( -0.1253332335642912687, 0.9921147013144795412, 0.000000000000000000 ) ) ;
#9712 = AXIS2_PLACEMENT_3D ( 'NONE', #9271, #13193, #21164 ) ;
#9713 = AXIS2_PLACEMENT_3D ( 'NONE', #15552, #17640, #21817 ) ;
#9714 = ORIENTED_EDGE ( 'NONE', *, *, #10693, .F. ) ;
#9715 = CARTESIAN_POINT ( 'NONE',  ( -1.999999999999998224, 27.10000000000000142, 12.46410161513774639 ) ) ;
#9716 = CYLINDRICAL_SURFACE ( 'NONE', #25599, 5.500000000000000000 ) ;
#9717 = CARTESIAN_POINT ( 'NONE',  ( 3.756430356250003655, -8.999999999999992895, 0.2531249993854844949 ) ) ;
#9718 = DIRECTION ( 'NONE',  ( 0.000000000000000000, 0.000000000000000000, 1.000000000000000000 ) ) ;
#9719 = CARTESIAN_POINT ( 'NONE',  ( 20.48178985837210320, 20.48178985837202859, 4.662447845253954171 ) ) ;
#9720 = EDGE_CURVE ( 'NONE', #5290, #15106, #23001, .T. ) ;
#9721 = FACE_OUTER_BOUND ( 'NONE', #381, .T. ) ;
#9722 = ADVANCED_FACE ( 'NONE', ( #7873 ), #14032, .T. ) ;
#9723 = CARTESIAN_POINT ( 'NONE',  ( -9.296355089585909904E-15, 29.10624999877097352, 4.999999999999992006 ) ) ;
#9724 = CARTESIAN_POINT ( 'NONE',  ( 4.000000000000001776, 29.01249999999999929, 11.30940107675849760 ) ) ;
#9725 = DIRECTION ( 'NONE',  ( 1.000000000000000000, 0.000000000000000000, 0.000000000000000000 ) ) ;
#9726 = VECTOR ( 'NONE', #2169, 1000.000000000000000 ) ;
#9727 = CARTESIAN_POINT ( 'NONE',  ( 19.28627369086489551, 21.94247106882419729, 12.25316411605951927 ) ) ;
#9728 = CARTESIAN_POINT ( 'NONE',  ( 2.900000000000003464, -8.999999999999992895, -10.00000000000000000 ) ) ;
#9729 = VERTEX_POINT ( 'NONE', #16123 ) ;
#9730 = EDGE_LOOP ( 'NONE', ( #21499, #20363, #15304, #20579 ) ) ;
#9731 = CARTESIAN_POINT ( 'NONE',  ( 1.878215178125005158, 25.77812499938548996, 5.746835883940462963 ) ) ;
#9732 = EDGE_CURVE ( 'NONE', #17145, #1087, #14676, .T. ) ;
#9733 = ORIENTED_EDGE ( 'NONE', *, *, #7770, .F. ) ;
#9734 = DIRECTION ( 'NONE',  ( 1.000000000000000000, 0.000000000000000000, 0.000000000000000000 ) ) ;
#9735 = VECTOR ( 'NONE', #11661, 1000.000000000000000 ) ;
#9736 = EDGE_LOOP ( 'NONE', ( #25175, #1836, #10565, #7543 ) ) ;
#9737 = ORIENTED_EDGE ( 'NONE', *, *, #1964, .F. ) ;
#9738 = VECTOR ( 'NONE', #6849, 1000.000000000000000 ) ;
#9739 = DIRECTION ( 'NONE',  ( -0.000000000000000000, 0.000000000000000000, 1.000000000000000000 ) ) ;
#9740 = ORIENTED_EDGE ( 'NONE', *, *, #107, .T. ) ;
#9741 = CARTESIAN_POINT ( 'NONE',  ( 3.100771756283734248, 38.96317070936194682, 4.412623259661243580 ) ) ;
#9742 = DIRECTION ( 'NONE',  ( 0.000000000000000000, 0.000000000000000000, -1.000000000000000000 ) ) ;
#9743 = CARTESIAN_POINT ( 'NONE',  ( 4.006172263299091013E-15, 28.40312499938548996, 4.662447845253954171 ) ) ;
#9744 = CARTESIAN_POINT ( 'NONE',  ( -4.000000000000001776, -26.76250000000000284, 11.30940107675849760 ) ) ;
#9745 = CARTESIAN_POINT ( 'NONE',  ( -1.999999999999994893, 27.85000000000000497, 5.535898384862237620 ) ) ;
#9746 = DIRECTION ( 'NONE',  ( 0.000000000000000000, 1.000000000000000000, -0.000000000000000000 ) ) ;
#9747 = SURFACE_STYLE_USAGE ( .BOTH. , #19679 ) ;
#9748 = CARTESIAN_POINT ( 'NONE',  ( -3.999999999999996447, -8.999999999999992895, 1.068749998770966103 ) ) ;
#9749 = AXIS2_PLACEMENT_3D ( 'NONE', #4944, #904, #8885 ) ;
#9750 = EDGE_CURVE ( 'NONE', #1796, #8646, #1725, .T. ) ;
#9751 = CARTESIAN_POINT ( 'NONE',  ( 31.09598070739550479, -0.4999838450260851164, -6.500000000000000000 ) ) ;
#9752 = CARTESIAN_POINT ( 'NONE',  ( 15.64473753375240506, 21.30159178324472080, 8.999999999999992895 ) ) ;
#9753 = CARTESIAN_POINT ( 'NONE',  ( 19.49840572522085935, 22.15460310318015758, 5.746835883940462963 ) ) ;
#9754 = CARTESIAN_POINT ( 'NONE',  ( -4.000000000000003553, -29.73213749463701561, 8.999999999999992895 ) ) ;
#9755 =( BOUNDED_CURVE ( )  B_SPLINE_CURVE ( 2, ( #22099, #4188, #5757, #20264, #18194, #279, #14011 ),
 .UNSPECIFIED., .F., .F. ) 
 B_SPLINE_CURVE_WITH_KNOTS ( ( 3, 2, 2, 3 ),
 ( 0.3500000000000000888, 0.3666666666666666963, 0.3833333333333333592, 0.3999999999999999667 ),
 .UNSPECIFIED. ) 
 CURVE ( )  GEOMETRIC_REPRESENTATION_ITEM ( )  RATIONAL_B_SPLINE_CURVE ( ( 0.9999999999999991118, 0.8660254037844395958, 1.000000000000000000, 0.8660254037844387076, 1.000000000000000000, 0.8660254037844391517, 0.9999999999999995559 ) ) 
 REPRESENTATION_ITEM ( '' )  );
#9756 = CARTESIAN_POINT ( 'NONE',  ( -1.878215178124998497, 29.49062499938548498, 12.25316411605951927 ) ) ;
#9757 = CARTESIAN_POINT ( 'NONE',  ( 22.10958068494259621, 20.27866814047594346, 5.206367449752296039 ) ) ;
#9758 = LINE ( 'NONE', #5963, #3319 ) ;
#9759 = FACE_OUTER_BOUND ( 'NONE', #15058, .T. ) ;
#9760 = ORIENTED_EDGE ( 'NONE', *, *, #21035, .T. ) ;
#9761 = CARTESIAN_POINT ( 'NONE',  ( -1.999999999999995781, 28.24374999877096570, 5.535898384862237620 ) ) ;
#9762 = CARTESIAN_POINT ( 'NONE',  ( 3.999999999999997335, -27.06250000000000000, 11.30940107675849404 ) ) ;
#9764 = ORIENTED_EDGE ( 'NONE', *, *, #19449, .F. ) ;
#9763 = CARTESIAN_POINT ( 'NONE',  ( -3.756430356249996549, 25.47812499938548925, 8.999999999999992895 ) ) ;
#9765 = EDGE_CURVE ( 'NONE', #5385, #13208, #6555, .T. ) ;
#9766 = CARTESIAN_POINT ( 'NONE',  ( -3.756430356249996994, 29.07812499938548356, 8.999999999999992895 ) ) ;
#9767 =( BOUNDED_CURVE ( )  B_SPLINE_CURVE ( 2, ( #827, #12600, #20706 ),
 .UNSPECIFIED., .F., .F. ) 
 B_SPLINE_CURVE_WITH_KNOTS ( ( 3, 3 ),
 ( 0.9889400238386636399, 1.000000000000000000 ),
 .UNSPECIFIED. ) 
 CURVE ( )  GEOMETRIC_REPRESENTATION_ITEM ( )  RATIONAL_B_SPLINE_CURVE ( ( 0.9401842259098239785, 0.9110946495778740051, 1.000000000000000000 ) ) 
 REPRESENTATION_ITEM ( '' )  );
#9768 = DIRECTION ( 'NONE',  ( 0.000000000000000000, 0.000000000000000000, 1.000000000000000000 ) ) ;
#9769 = CARTESIAN_POINT ( 'NONE',  ( 3.403349963601422168, 25.83240171513484285, 20.00001200000000523 ) ) ;
#9770 = CARTESIAN_POINT ( 'NONE',  ( -31.10000000000000142, 3.257552089140643357E-13, -6.500000000000000000 ) ) ;
#9771 = ORIENTED_EDGE ( 'NONE', *, *, #20313, .F. ) ;
#9772 = ORIENTED_EDGE ( 'NONE', *, *, #24990, .F. ) ;
#9773 = DIRECTION ( 'NONE',  ( -0.000000000000000000, 0.000000000000000000, -1.000000000000000000 ) ) ;
#9774 = CARTESIAN_POINT ( 'NONE',  ( -3.756430356249994773, 25.81562499938548783, 8.999999999999992895 ) ) ;
#9775 = CARTESIAN_POINT ( 'NONE',  ( 3.756430356250003211, -6.831223922626973533, 3.328124999385480898 ) ) ;
#9776 = CARTESIAN_POINT ( 'NONE',  ( -16.23990935651680445, 26.52310962334767908, -2.750000000000000000 ) ) ;
#9777 = FACE_OUTER_BOUND ( 'NONE', #5281, .T. ) ;
#9778 = DIRECTION ( 'NONE',  ( 0.000000000000000000, 0.000000000000000000, 1.000000000000000000 ) ) ;
#9779 = CARTESIAN_POINT ( 'NONE',  ( 20.73590635829554429, 17.90747923354928162, 5.535898384862238508 ) ) ;
#9780 = CARTESIAN_POINT ( 'NONE',  ( -3.999999999999997335, 26.61250000000000071, 11.30940107675849404 ) ) ;
#9781 = CARTESIAN_POINT ( 'NONE',  ( 5.577813053751546416E-15, 25.73124999877097352, 12.99999999999999289 ) ) ;
#9782 = CARTESIAN_POINT ( 'NONE',  ( 20.77801835412135745, 15.46562359820254784, 6.831223922626973533 ) ) ;
#9783 = CARTESIAN_POINT ( 'NONE',  ( 16.26787538380399312, 21.92472963329630176, 11.30940107675849404 ) ) ;
#9784 = ORIENTED_EDGE ( 'NONE', *, *, #11186, .F. ) ;
#9785 = CARTESIAN_POINT ( 'NONE',  ( -5.532151103383211144, 38.49999999999999289, 11.32277940608570255 ) ) ;
#9786 = CARTESIAN_POINT ( 'NONE',  ( 0.5258040994055174222, 29.99650528990839859, 5.025965267902964939 ) ) ;
#9787 = CARTESIAN_POINT ( 'NONE',  ( -1.878215178124998497, 28.25312499938548427, 12.25316411605951927 ) ) ;
#9789 = ADVANCED_FACE ( 'NONE', ( #12716 ), #14537, .T. ) ;
#9788 = CARTESIAN_POINT ( 'NONE',  ( -27.25313774936397948, 14.98253926456367502, 1.000000000000000000 ) ) ;
#9790 = CARTESIAN_POINT ( 'NONE',  ( -5.327558883615603591, 30.54913349766230724, 1.000000000000000000 ) ) ;
#9791 = DIRECTION ( 'NONE',  ( 0.000000000000000000, 0.000000000000000000, 1.000000000000000000 ) ) ;
#9792 = EDGE_LOOP ( 'NONE', ( #186, #29, #20419, #2920 ) ) ;
#9793 = CARTESIAN_POINT ( 'NONE',  ( 2.451530025008918923, -31.00322564728515928, -2.750000000000000000 ) ) ;
#9794 = CARTESIAN_POINT ( 'NONE',  ( -28.14012133169306296, 13.24173596767408867, -6.500000000000000000 ) ) ;
#9796 = VERTEX_POINT ( 'NONE', #14422 ) ;
#9795 = CARTESIAN_POINT ( 'NONE',  ( 4.000000000000003553, 28.54374999877097707, 8.999999999999992895 ) ) ;
#9797 = ADVANCED_FACE ( 'NONE', ( #18215 ), #14155, .T. ) ;
#9798 = EDGE_LOOP ( 'NONE', ( #11963, #12002, #24756, #22827 ) ) ;
#9799 = ORIENTED_EDGE ( 'NONE', *, *, #7902, .F. ) ;
#9800 = ORIENTED_EDGE ( 'NONE', *, *, #15969, .F. ) ;
#9801 = EDGE_CURVE ( 'NONE', #19150, #23030, #12190, .T. ) ;
#9802 = ORIENTED_EDGE ( 'NONE', *, *, #7229, .F. ) ;
#9803 = CARTESIAN_POINT ( 'NONE',  ( 21.21320343559646915, 21.21320343559638744, 8.999999999999992895 ) ) ;
#9804 = CARTESIAN_POINT ( 'NONE',  ( -3.834746474454188013E-15, -28.20624999877096428, 4.999999999999992006 ) ) ;
#9805 = SURFACE_STYLE_USAGE ( .BOTH. , #21961 ) ;
#9806 = CARTESIAN_POINT ( 'NONE',  ( -2.003086131649545506E-15, 27.27812499938548640, 13.33755215474602984 ) ) ;
#9807 = CARTESIAN_POINT ( 'NONE',  ( 3.735045420075836212E-15, -4.662447845253954171, 2.503124999385483385 ) ) ;
#9808 = CARTESIAN_POINT ( 'NONE',  ( 2.000000000000003997, -5.535898384862238508, 3.168749998770967302 ) ) ;
#9809 = CARTESIAN_POINT ( 'NONE',  ( 20.51285331117640709, 15.20045855525759393, 8.999999999999992895 ) ) ;
#9810 = CARTESIAN_POINT ( 'NONE',  ( 1.878215178125000939, 29.22812499938548569, 12.25316411605952283 ) ) ;
#9811 = LINE ( 'NONE', #14262, #23836 ) ;
#9812 = DIRECTION ( 'NONE',  ( 0.000000000000000000, 0.000000000000000000, 1.000000000000000000 ) ) ;
#9813 = CARTESIAN_POINT ( 'NONE',  ( -1.999999999999995781, -5.535898384862237620, 1.049999999999998934 ) ) ;
#9814 = CARTESIAN_POINT ( 'NONE',  ( -23.01025686871661335, -20.92219106202025714, -2.750000000000000000 ) ) ;
#9815 = CARTESIAN_POINT ( 'NONE',  ( -19.43607991389006528, -24.27856662945486832, -2.750000000000000000 ) ) ;
#9816 = CARTESIAN_POINT ( 'NONE',  ( 3.999999999999996003, -27.83124999877096784, 6.690598923241487306 ) ) ;
#9817 = CARTESIAN_POINT ( 'NONE',  ( 3.756430356250002323, 27.91562499938548569, 11.16877607737301226 ) ) ;
#9818 = FACE_OUTER_BOUND ( 'NONE', #2981, .T. ) ;
#9819 = DIRECTION ( 'NONE',  ( 0.9510565162951586382, 0.3090169943749320192, 0.000000000000000000 ) ) ;
#9820 = DIRECTION ( 'NONE',  ( 0.000000000000000000, 0.000000000000000000, 1.000000000000000000 ) ) ;
#9822 = ORIENTED_EDGE ( 'NONE', *, *, #18741, .T. ) ;
#9821 = PRODUCT_DEFINITION ( 'UNKNOWN', '', #7690, #23252 ) ;
#9823 = DIRECTION ( 'NONE',  ( 0.000000000000000000, 0.000000000000000000, 1.000000000000000000 ) ) ;
#9824 = ORIENTED_EDGE ( 'NONE', *, *, #24086, .T. ) ;
#9825 = ORIENTED_EDGE ( 'NONE', *, *, #23587, .F. ) ;
#9826 = LINE ( 'NONE', #17811, #5377 ) ;
#9827 = ORIENTED_EDGE ( 'NONE', *, *, #12249, .F. ) ;
#9828 = CARTESIAN_POINT ( 'NONE',  ( 3.756430356249996994, -27.27812499938548640, 8.999999999999992895 ) ) ;
#9829 = EDGE_CURVE ( 'NONE', #6029, #6210, #9222, .T. ) ;
#9830 = ORIENTED_EDGE ( 'NONE', *, *, #17987, .F. ) ;
#9831 = DIRECTION ( 'NONE',  ( 0.000000000000000000, 0.000000000000000000, 1.000000000000000000 ) ) ;
#9832 = EDGE_CURVE ( 'NONE', #23923, #15811, #7553, .T. ) ;
#9833 = ORIENTED_EDGE ( 'NONE', *, *, #10998, .T. ) ;
#9834 = CARTESIAN_POINT ( 'NONE',  ( 3.752267015613588906E-15, 28.71250000000000568, 4.381197846482986158 ) ) ;
#9835 = DIRECTION ( 'NONE',  ( -0.000000000000000000, -1.000000000000000000, -0.000000000000000000 ) ) ;
#9836 = CARTESIAN_POINT ( 'NONE',  ( -1.878215178124995832, -5.746835883940462963, 0.4031249993854852942 ) ) ;
#9837 = DIRECTION ( 'NONE',  ( 0.000000000000000000, 0.000000000000000000, -1.000000000000000000 ) ) ;
#9838 = PRODUCT_DEFINITION_SHAPE ( 'NONE', 'NONE',  #13015 ) ;
#9839 = CARTESIAN_POINT ( 'NONE',  ( 18.24985654912466515, 23.56225130504333976, 11.16877607737301226 ) ) ;
#9840 = DIRECTION ( 'NONE',  ( 1.000000000000000000, 0.000000000000000000, 0.000000000000000000 ) ) ;
#9841 = CYLINDRICAL_SURFACE ( 'NONE', #15061, 0.5000000000000004441 ) ;
#9842 = PRODUCT_CONTEXT ( 'NONE', #17136, 'mechanical' ) ;
#9843 = CARTESIAN_POINT ( 'NONE',  ( 4.000000000000003553, 27.28749999999999787, 6.690598923241489970 ) ) ;
#9844 = DIRECTION ( 'NONE',  ( 0.000000000000000000, 0.000000000000000000, -1.000000000000000000 ) ) ;
#9845 = CARTESIAN_POINT ( 'NONE',  ( 22.76675617620853131, 17.45436142028971460, 6.831223922626973533 ) ) ;
#9846 = DIRECTION ( 'NONE',  ( 0.6845471059286972748, 0.7289686274214034478, 0.000000000000000000 ) ) ;
#9847 = CIRCLE ( 'NONE', #24037, 31.10000000000000142 ) ;
#9848 = ORIENTED_EDGE ( 'NONE', *, *, #23472, .T. ) ;
#9849 = ORIENTED_EDGE ( 'NONE', *, *, #11499, .F. ) ;
#9850 = CARTESIAN_POINT ( 'NONE',  ( -3.756430356249998326, 25.51562499938549067, 11.16877607737301226 ) ) ;
#9851 = EDGE_LOOP ( 'NONE', ( #305, #6351, #20244, #15774 ) ) ;
#9852 = LINE ( 'NONE', #17835, #16694 ) ;
#9853 = EDGE_CURVE ( 'NONE', #17013, #18550, #20161, .T. ) ;
#9854 = CARTESIAN_POINT ( 'NONE',  ( -3.756430356249997882, 26.86562499938548498, 11.16877607737301226 ) ) ;
#9855 = CARTESIAN_POINT ( 'NONE',  ( -3.756430356249997882, 29.11562499938548143, 11.16877607737301226 ) ) ;
#9856 = CARTESIAN_POINT ( 'NONE',  ( 4.000000000000003553, 28.13124999877096855, 6.690598923241489970 ) ) ;
#9857 = ORIENTED_EDGE ( 'NONE', *, *, #22807, .F. ) ;
#9858 = ORIENTED_EDGE ( 'NONE', *, *, #15600, .T. ) ;
#9859 = ADVANCED_FACE ( 'NONE', ( #6305 ), #22516, .F. ) ;
#9860 = CARTESIAN_POINT ( 'NONE',  ( 1.999999999999995781, -25.60000000000000142, 5.535898384862237620 ) ) ;
#9861 = ORIENTED_EDGE ( 'NONE', *, *, #998, .F. ) ;
#9862 = LINE ( 'NONE', #3710, #25601 ) ;
#9863 = FACE_OUTER_BOUND ( 'NONE', #15185, .T. ) ;
#9864 = CARTESIAN_POINT ( 'NONE',  ( 1.878215178125003382, 28.36562499938548498, 5.746835883940462963 ) ) ;
#9865 = CARTESIAN_POINT ( 'NONE',  ( 0.000000000000000000, 0.000000000000000000, -6.500000000000000000 ) ) ;
#9866 = CARTESIAN_POINT ( 'NONE',  ( 2.000000000000005329, 27.77500000000000568, 5.535898384862238508 ) ) ;
#9867 = EDGE_CURVE ( 'NONE', #4609, #2753, #24668, .T. ) ;
#9868 = CARTESIAN_POINT ( 'NONE',  ( 2.672651547586948120E-15, 26.37812499938548427, 13.33755215474602984 ) ) ;
#9869 = CARTESIAN_POINT ( 'NONE',  ( 3.999999999999995559, -28.73124999877096997, 6.690598923241487306 ) ) ;
#9870 = CARTESIAN_POINT ( 'NONE',  ( 1.859271017917182139E-15, 27.08124999877096784, 12.99999999999999289 ) ) ;
#9871 = CARTESIAN_POINT ( 'NONE',  ( 17.64231419060439876, 20.47074131535051933, 5.535898384862237620 ) ) ;
#9872 = CARTESIAN_POINT ( 'NONE',  ( 18.64987758779700044, 21.30607496575630222, 12.25316411605951927 ) ) ;
#9873 = CARTESIAN_POINT ( 'NONE',  ( -4.000000000000001776, -28.50624999877096855, 11.30940107675849760 ) ) ;
#9874 = CARTESIAN_POINT ( 'NONE',  ( 4.000000000000001776, 29.40624999877096357, 11.30940107675849760 ) ) ;
#9875 = CARTESIAN_POINT ( 'NONE',  ( -22.17092431280563503, 21.28941499438250062, 1.000000000000000000 ) ) ;
#9876 = DIRECTION ( 'NONE',  ( -0.6845471059286831750, 0.7289686274214168815, 0.000000000000000000 ) ) ;
#9877 = CARTESIAN_POINT ( 'NONE',  ( 1.071796769724495446, 25.93615380933863790, 4.999999999999992895 ) ) ;
#9878 = ORIENTED_EDGE ( 'NONE', *, *, #4843, .F. ) ;
#9879 = CARTESIAN_POINT ( 'NONE',  ( 4.000000000000003553, 28.58124999877096784, 6.690598923241489970 ) ) ;
#9880 = CARTESIAN_POINT ( 'NONE',  ( -3.752267015613588906E-15, -26.91250000000000142, 4.381197846482986158 ) ) ;
#9882 = ORIENTED_EDGE ( 'NONE', *, *, #16665, .T. ) ;
#9881 = CARTESIAN_POINT ( 'NONE',  ( 4.000000000000003553, 29.50000000000000355, 8.999999999999992895 ) ) ;
#9883 = CARTESIAN_POINT ( 'NONE',  ( -1.878215178124998497, 29.60312499938548569, 12.25316411605951927 ) ) ;
#9884 = CARTESIAN_POINT ( 'NONE',  ( 3.469446951953614189E-15, -8.999999999999992895, 6.000000000000000000 ) ) ;
#9885 = CARTESIAN_POINT ( 'NONE',  ( -8.377607117416806304, 24.67207871933483787, 20.00001200000000168 ) ) ;
#9886 = CARTESIAN_POINT ( 'NONE',  ( -26.50000000000000355, 0.5000000000000000000, 19.50000000000000000 ) ) ;
#9887 = ORIENTED_EDGE ( 'NONE', *, *, #24881, .T. ) ;
#9888 = ORIENTED_EDGE ( 'NONE', *, *, #5167, .F. ) ;
#9889 = CARTESIAN_POINT ( 'NONE',  ( -0.4999838450259764255, 31.09598070739550124, -6.500000000000000000 ) ) ;
#9890 = CARTESIAN_POINT ( 'NONE',  ( -1.878215178124998275, 25.89062499938549067, 12.25316411605951927 ) ) ;
#9891 = EDGE_CURVE ( 'NONE', #24264, #14407, #296, .T. ) ;
#9892 = CARTESIAN_POINT ( 'NONE',  ( 3.735045420075836212E-15, -4.662447845253954171, 4.303124999385482319 ) ) ;
#9893 = CARTESIAN_POINT ( 'NONE',  ( 3.834746474454188013E-15, 25.56250000000000000, 4.999999999999992006 ) ) ;
#9894 =( BOUNDED_CURVE ( )  B_SPLINE_CURVE ( 2, ( #6701, #14436, #6320, #581, #22676 ),
 .UNSPECIFIED., .F., .F. ) 
 B_SPLINE_CURVE_WITH_KNOTS ( ( 3, 2, 3 ),
 ( 0.000000000000000000, 0.01666666666666666644, 0.02500000000000000486 ),
 .UNSPECIFIED. ) 
 CURVE ( )  GEOMETRIC_REPRESENTATION_ITEM ( )  RATIONAL_B_SPLINE_CURVE ( ( 1.000000000000000000, 0.8660254037844387076, 1.000000000000000000, 0.9330127018922194093, 0.9330127018922194093 ) ) 
 REPRESENTATION_ITEM ( '' )  );
#9895 = CARTESIAN_POINT ( 'NONE',  ( 0.000000000000000000, 0.000000000000000000, -6.500000000000000000 ) ) ;
#9896 = DIRECTION ( 'NONE',  ( 0.000000000000000000, 0.000000000000000000, 1.000000000000000000 ) ) ;
#9897 = LINE ( 'NONE', #12255, #21361 ) ;
#9898 = CARTESIAN_POINT ( 'NONE',  ( 21.12923450446149687, 15.47238025496904612, 6.690598923241489970 ) ) ;
#9899 = FACE_OUTER_BOUND ( 'NONE', #16336, .T. ) ;
#9900 = CARTESIAN_POINT ( 'NONE',  ( 3.469446951953614189E-15, 31.50000000000000000, 8.999999999999992895 ) ) ;
#9901 = CARTESIAN_POINT ( 'NONE',  ( 19.63547142920491595, 16.80704430445866393, 12.46410161513774817 ) ) ;
#9902 = ORIENTED_EDGE ( 'NONE', *, *, #15885, .F. ) ;
#9903 = CARTESIAN_POINT ( 'NONE',  ( -8.831537335106614961E-15, -27.13750000000000284, 12.99999999999999112 ) ) ;
#9904 = CARTESIAN_POINT ( 'NONE',  ( 5.606326150107658890, 38.73250905386370135, 7.645898033760625268 ) ) ;
#9905 =( BOUNDED_CURVE ( )  B_SPLINE_CURVE ( 2, ( #23493, #3872, #17738, #7790, #3731 ),
 .UNSPECIFIED., .F., .F. ) 
 B_SPLINE_CURVE_WITH_KNOTS ( ( 3, 2, 3 ),
 ( 0.000000000000000000, 0.01666666666666666644, 0.02500000000000001180 ),
 .UNSPECIFIED. ) 
 CURVE ( )  GEOMETRIC_REPRESENTATION_ITEM ( )  RATIONAL_B_SPLINE_CURVE ( ( 1.000000000000000000, 0.8660254037844387076, 1.000000000000000000, 0.9330127018922191873, 0.9330127018922192983 ) ) 
 REPRESENTATION_ITEM ( '' )  );
#9906 = CARTESIAN_POINT ( 'NONE',  ( 3.756430356250003655, 27.05312499938548498, 8.999999999999992895 ) ) ;
#9907 = LINE ( 'NONE', #23393, #12042 ) ;
#9908 = CARTESIAN_POINT ( 'NONE',  ( -30.45149776762723448, 6.317933499823641164, 1.000000000000000000 ) ) ;
#9909 = CARTESIAN_POINT ( 'NONE',  ( 21.21320343559646915, 21.21320343559638744, 4.999999999999992006 ) ) ;
#9910 = ORIENTED_EDGE ( 'NONE', *, *, #11672, .T. ) ;
#9911 = DIRECTION ( 'NONE',  ( 0.000000000000000000, -1.000000000000000000, 0.000000000000000000 ) ) ;
#9912 = CARTESIAN_POINT ( 'NONE',  ( -10.08469938919519926, -29.41953157733083302, -2.750000000000000000 ) ) ;
#9914 = ORIENTED_EDGE ( 'NONE', *, *, #17759, .F. ) ;
#9913 = CARTESIAN_POINT ( 'NONE',  ( -30.12293631110035363, 7.734255490827311341, -6.500000000000000000 ) ) ;
#9915 = ORIENTED_EDGE ( 'NONE', *, *, #18201, .F. ) ;
#9916 = ORIENTED_EDGE ( 'NONE', *, *, #4755, .T. ) ;
#9917 = ORIENTED_EDGE ( 'NONE', *, *, #4034, .F. ) ;
#9918 = CARTESIAN_POINT ( 'NONE',  ( -3.897863563849436552, 30.85476721088031482, 1.000000000000000000 ) ) ;
#9919 = CARTESIAN_POINT ( 'NONE',  ( -4.000000000000003553, -29.73213749463701561, 8.999999999999992895 ) ) ;
#9920 = EDGE_CURVE ( 'NONE', #22706, #24134, #25795, .T. ) ;
#9921 = VECTOR ( 'NONE', #3185, 1000.000000000000000 ) ;
#9922 = CARTESIAN_POINT ( 'NONE',  ( 1.878215178125001605, 27.31562499938548783, 12.25316411605952283 ) ) ;
#9923 = EDGE_CURVE ( 'NONE', #13585, #1315, #10336, .T. ) ;
#9924 = CARTESIAN_POINT ( 'NONE',  ( 3.756430356250002323, -11.16877607737301226, 2.353124999385479477 ) ) ;
#9925 = CARTESIAN_POINT ( 'NONE',  ( 4.000000000000003553, -6.690598923241489970, 4.481249998770969079 ) ) ;
#9926 =( LENGTH_UNIT ( ) NAMED_UNIT ( * ) SI_UNIT ( .MILLI., .METRE. ) );
#9927 = ADVANCED_FACE ( 'NONE', ( #2646 ), #24357, .F. ) ;
#9928 = CARTESIAN_POINT ( 'NONE',  ( -3.756430356249996994, 27.27812499938548640, 8.999999999999992895 ) ) ;
#9929 = CARTESIAN_POINT ( 'NONE',  ( 18.92274273964848064, 20.43849226750045389, 4.999999999999992006 ) ) ;
#9930 = CARTESIAN_POINT ( 'NONE',  ( 1.000000000000000000, 0.000000000000000000, 19.50000000000000000 ) ) ;
#9931 = CARTESIAN_POINT ( 'NONE',  ( -3.999999999999996003, -6.690598923241487306, 1.987499999999999600 ) ) ;
#9932 =( REPRESENTATION_RELATIONSHIP ('NONE','NONE', #25031, #23199 ) REPRESENTATION_RELATIONSHIP_WITH_TRANSFORMATION ( #688 )SHAPE_REPRESENTATION_RELATIONSHIP( ) );
#9933 = CYLINDRICAL_SURFACE ( 'NONE', #17567, 4.000000000000000000 ) ;
#9935 = ADVANCED_FACE ( 'NONE', ( #2859 ), #3000, .T. ) ;
#9934 = DIRECTION ( 'NONE',  ( 0.000000000000000000, 1.000000000000000000, -0.000000000000000000 ) ) ;
#9936 = DIRECTION ( 'NONE',  ( 0.000000000000000000, 0.000000000000000000, 1.000000000000000000 ) ) ;
#9937 = CARTESIAN_POINT ( 'NONE',  ( 3.999999999999996447, -29.66874999877096997, 8.999999999999992895 ) ) ;
#9938 = CARTESIAN_POINT ( 'NONE',  ( -3.756430356249995661, 27.24062499938548498, 6.831223922626973533 ) ) ;
#9939 = DIRECTION ( 'NONE',  ( 0.000000000000000000, 0.000000000000000000, 1.000000000000000000 ) ) ;
#9940 = CIRCLE ( 'NONE', #766, 0.5000000000000003331 ) ;
#9941 = DIRECTION ( 'NONE',  ( 0.000000000000000000, 0.000000000000000000, -1.000000000000000000 ) ) ;
#9942 = CARTESIAN_POINT ( 'NONE',  ( 1.626862140677534194E-14, 28.03750000000000497, 12.99999999999999289 ) ) ;
#9943 = ORIENTED_EDGE ( 'NONE', *, *, #6789, .T. ) ;
#9944 = CARTESIAN_POINT ( 'NONE',  ( 7.437084071668728555E-15, 27.13750000000000639, 12.99999999999999112 ) ) ;
#9946 = ORIENTED_EDGE ( 'NONE', *, *, #3720, .F. ) ;
#9945 = CARTESIAN_POINT ( 'NONE',  ( 3.834746474454188013E-15, 28.26249999999999929, 4.999999999999992006 ) ) ;
#9947 = ORIENTED_EDGE ( 'NONE', *, *, #6827, .F. ) ;
#9948 = CARTESIAN_POINT ( 'NONE',  ( -3.999999999999996447, -8.999999999999992895, 1.518749998770968501 ) ) ;
#9950 = ORIENTED_EDGE ( 'NONE', *, *, #8784, .T. ) ;
#9949 = CIRCLE ( 'NONE', #7017, 0.5000000000000004441 ) ;
#9951 = CARTESIAN_POINT ( 'NONE',  ( -3.756430356250004099, -26.07812499938548356, 6.831223922626973533 ) ) ;
#9952 = VERTEX_POINT ( 'NONE', #10444 ) ;
#9953 = DIRECTION ( 'NONE',  ( -0.000000000000000000, -1.000000000000000000, -0.000000000000000000 ) ) ;
#9954 = ORIENTED_EDGE ( 'NONE', *, *, #314, .F. ) ;
#9955 = CARTESIAN_POINT ( 'NONE',  ( -3.999999999999996003, 28.78750000000000142, 6.690598923241487306 ) ) ;
#9956 = CARTESIAN_POINT ( 'NONE',  ( -3.756430356249996105, 26.34062499938548285, 6.831223922626973533 ) ) ;
#9957 = AXIS2_PLACEMENT_3D ( 'NONE', #22981, #10940, #24539 ) ;
#9958 = CARTESIAN_POINT ( 'NONE',  ( -3.756430356249997882, -11.16877607737301226, 1.415624999385483029 ) ) ;
#9959 = AXIS2_PLACEMENT_3D ( 'NONE', #6237, #2321, #3898 ) ;
#9960 = DIRECTION ( 'NONE',  ( 0.000000000000000000, 0.000000000000000000, 1.000000000000000000 ) ) ;
#9961 = CARTESIAN_POINT ( 'NONE',  ( 19.28854716511979461, 19.28854716511973066, 13.33755215474602984 ) ) ;
#9962 = EDGE_CURVE ( 'NONE', #3427, #20963, #12746, .T. ) ;
#9963 = CARTESIAN_POINT ( 'NONE',  ( -29.07785765677936851, -9.610428525060582317, -6.500000000000000000 ) ) ;
#9964 = VECTOR ( 'NONE', #11793, 1000.000000000000000 ) ;
#9965 = AXIS2_PLACEMENT_3D ( 'NONE', #4958, #12939, #3003 ) ;
#9966 = EDGE_CURVE ( 'NONE', #22105, #25114, #8505, .T. ) ;
#9967 = CARTESIAN_POINT ( 'NONE',  ( -1.999999999999995781, 27.85000000000000142, 5.535898384862237620 ) ) ;
#9968 = EDGE_CURVE ( 'NONE', #16896, #3917, #4212, .T. ) ;
#9969 = DIRECTION ( 'NONE',  ( 0.000000000000000000, 0.000000000000000000, 1.000000000000000000 ) ) ;
#9970 = CARTESIAN_POINT ( 'NONE',  ( 21.67730602587931088, 19.02110864791986344, 12.25316411605952283 ) ) ;
#9971 = LINE ( 'NONE', #9728, #25848 ) ;
#9972 = VERTEX_POINT ( 'NONE', #2737 ) ;
#9973 = ORIENTED_EDGE ( 'NONE', *, *, #13013, .T. ) ;
#9974 = CARTESIAN_POINT ( 'NONE',  ( 3.756430356250003211, 25.70312499938548356, 8.999999999999992895 ) ) ;
#9975 = VERTEX_POINT ( 'NONE', #12409 ) ;
#9976 = CARTESIAN_POINT ( 'NONE',  ( 2.000000000000000888, 29.81874999877096855, 12.46410161513774817 ) ) ;
#9977 = CARTESIAN_POINT ( 'NONE',  ( 2.620986760973688460E-15, 29.78124999877096712, 13.61880215351699874 ) ) ;
#9978 = AXIS2_PLACEMENT_3D ( 'NONE', #15932, #10029, #12122 ) ;
#9979 = LINE ( 'NONE', #13921, #6776 ) ;
#9980 = VERTEX_POINT ( 'NONE', #4953 ) ;
#9981 = VECTOR ( 'NONE', #8487, 1000.000000000000000 ) ;
#9982 = LINE ( 'NONE', #16020, #1490 ) ;
#9983 = ORIENTED_EDGE ( 'NONE', *, *, #6110, .F. ) ;
#9984 = CARTESIAN_POINT ( 'NONE',  ( 0.2827178117968801030, 38.91165577845126222, 14.58153869134143577 ) ) ;
#9985 = CARTESIAN_POINT ( 'NONE',  ( -1.878215178124995832, 26.19062499938548427, 5.746835883940462963 ) ) ;
#9986 = CYLINDRICAL_SURFACE ( 'NONE', #1807, 31.10000000000000142 ) ;
#9987 = CARTESIAN_POINT ( 'NONE',  ( 0.4949451094549379704, 38.61079987549954495, 3.131633208832877102 ) ) ;
#9988 = DIRECTION ( 'NONE',  ( 1.000000000000000000, 0.000000000000000000, 0.000000000000000000 ) ) ;
#9989 = CARTESIAN_POINT ( 'NONE',  ( 0.000000000000000000, 26.23750000000000426, 13.61880215351699874 ) ) ;
#9990 = CIRCLE ( 'NONE', #420, 0.5000000000000017764 ) ;
#9991 = CARTESIAN_POINT ( 'NONE',  ( 3.756430356250003655, 26.04062499938548569, 8.999999999999992895 ) ) ;
#9992 = FILL_AREA_STYLE ('',( #22521 ) ) ;
#9994 = EDGE_CURVE ( 'NONE', #25291, #19323, #2131, .T. ) ;
#9993 = VECTOR ( 'NONE', #7749, 1000.000000000000000 ) ;
#9995 = CARTESIAN_POINT ( 'NONE',  ( 0.000000000000000000, 0.000000000000000000, 1.000000000000000000 ) ) ;
#9996 = CIRCLE ( 'NONE', #22948, 6.000000000000000000 ) ;
#9997 = DIRECTION ( 'NONE',  ( 0.000000000000000000, 0.000000000000000000, 1.000000000000000000 ) ) ;
#9998 = CARTESIAN_POINT ( 'NONE',  ( 17.23572779142213918, 22.89258204091444782, 8.999999999999992895 ) ) ;
#9999 = CARTESIAN_POINT ( 'NONE',  ( 22.31370212894720240, 19.65750475098775496, 12.25316411605952283 ) ) ;
#10000 = CARTESIAN_POINT ( 'NONE',  ( -4.000000000000002665, -29.73213749463701205, 9.470295877454901756 ) ) ;
#10001 = EDGE_CURVE ( 'NONE', #13400, #15214, #10576, .T. ) ;
#10002 = CARTESIAN_POINT ( 'NONE',  ( 0.000000000000000000, 0.000000000000000000, -6.500000000000000000 ) ) ;
#10003 = CARTESIAN_POINT ( 'NONE',  ( -1.878215178125000939, -25.96562499938548285, 12.25316411605952283 ) ) ;
#10004 = CARTESIAN_POINT ( 'NONE',  ( 21.91595456452976975, 19.25975718657032232, 12.25316411605952283 ) ) ;
#10005 = CIRCLE ( 'NONE', #14606, 0.4999999999999992784 ) ;
#10006 = ORIENTED_EDGE ( 'NONE', *, *, #13200, .F. ) ;
#10007 = CARTESIAN_POINT ( 'NONE',  ( 2.000000000000000888, 27.11874999877096926, 12.46410161513774817 ) ) ;
#10008 = CARTESIAN_POINT ( 'NONE',  ( -2.000000000000003997, -27.77500000000000213, 5.535898384862238508 ) ) ;
#10010 = ORIENTED_EDGE ( 'NONE', *, *, #17656, .F. ) ;
#10009 = CARTESIAN_POINT ( 'NONE',  ( -3.756430356249996549, 26.82812499938549067, 8.999999999999992895 ) ) ;
#10011 = CARTESIAN_POINT ( 'NONE',  ( -3.756430356249996994, 28.17812499938548498, 8.999999999999992895 ) ) ;
#10012 = CARTESIAN_POINT ( 'NONE',  ( -29.72853858738272592, 9.133673601486785643, -6.500000000000000000 ) ) ;
#10013 =( BOUNDED_CURVE ( )  B_SPLINE_CURVE ( 2, ( #25580, #7665, #23615, #9874, #25830, #7915, #5694, #15901, #11960 ),
 .UNSPECIFIED., .F., .F. ) 
 B_SPLINE_CURVE_WITH_KNOTS ( ( 3, 2, 2, 2, 3 ),
 ( 0.8750000000000000000, 0.8833333333333333037, 0.9000000000000000222, 0.9166666666666666297, 0.9250000000000000444 ),
 .UNSPECIFIED. ) 
 CURVE ( )  GEOMETRIC_REPRESENTATION_ITEM ( )  RATIONAL_B_SPLINE_CURVE ( ( 0.9330127018922194093, 0.9330127018922194093, 1.000000000000000000, 0.8660254037844387076, 1.000000000000000000, 0.8660254037844387076, 1.000000000000000000, 0.9330127018922189652, 0.9330127018922194093 ) ) 
 REPRESENTATION_ITEM ( '' )  );
#10014 = FACE_OUTER_BOUND ( 'NONE', #22250, .T. ) ;
#10015 = ORIENTED_EDGE ( 'NONE', *, *, #8660, .T. ) ;
#10016 = EDGE_LOOP ( 'NONE', ( #17710, #3146, #1165, #18973 ) ) ;
#10017 = CARTESIAN_POINT ( 'NONE',  ( -3.756430356249996105, 28.92812499938548498, 6.831223922626973533 ) ) ;
#10018 = AXIS2_PLACEMENT_3D ( 'NONE', #10606, #4594, #12714 ) ;
#10019 = CARTESIAN_POINT ( 'NONE',  ( -3.756430356249997438, -11.16877607737301048, 4.453124999385482674 ) ) ;
#10020 = CIRCLE ( 'NONE', #13789, 2.000000000000000000 ) ;
#10021 = LINE ( 'NONE', #2058, #25053 ) ;
#10022 = EDGE_CURVE ( 'NONE', #6810, #24237, #20071, .T. ) ;
#10023 = DIRECTION ( 'NONE',  ( 0.000000000000000000, 0.000000000000000000, 1.000000000000000000 ) ) ;
#10024 = CIRCLE ( 'NONE', #19236, 0.4999999999999996114 ) ;
#10025 = EDGE_CURVE ( 'NONE', #4416, #1143, #10887, .T. ) ;
#10026 = AXIS2_PLACEMENT_3D ( 'NONE', #1363, #17052, #25023 ) ;
#10027 = DIRECTION ( 'NONE',  ( 0.000000000000000000, 1.000000000000000000, 0.000000000000000000 ) ) ;
#10028 = CARTESIAN_POINT ( 'NONE',  ( 0.000000000000000000, 0.000000000000000000, -6.500000000000000000 ) ) ;
#10029 = DIRECTION ( 'NONE',  ( -0.000000000000000000, -0.000000000000000000, 1.000000000000000000 ) ) ;
#10030 = CARTESIAN_POINT ( 'NONE',  ( 17.84560739019554276, 23.50246163968784430, 6.690598923241487306 ) ) ;
#10031 = FACE_OUTER_BOUND ( 'NONE', #285, .T. ) ;
#10032 = CARTESIAN_POINT ( 'NONE',  ( 19.29959570814131808, 22.12802283288743155, 12.46410161513774639 ) ) ;
#10033 = VERTEX_POINT ( 'NONE', #8893 ) ;
#10034 = CARTESIAN_POINT ( 'NONE',  ( -5.221103800765325431, 38.91143067427094593, 10.99401152278178451 ) ) ;
#10035 = CARTESIAN_POINT ( 'NONE',  ( 0.000000000000000000, 0.000000000000000000, 1.000000000000000000 ) ) ;
#10036 = CARTESIAN_POINT ( 'NONE',  ( -3.756430356249997882, 28.21562499938548285, 11.16877607737301226 ) ) ;
#10037 = AXIS2_PLACEMENT_3D ( 'NONE', #2768, #14538, #22518 ) ;
#10038 = DIRECTION ( 'NONE',  ( -0.7071067811865487940, -0.7071067811865463515, 0.000000000000000000 ) ) ;
#10039 = DIRECTION ( 'NONE',  ( -0.000000000000000000, -0.000000000000000000, -1.000000000000000000 ) ) ;
#10040 = CARTESIAN_POINT ( 'NONE',  ( 2.000000000000003997, 29.06874999877096855, 5.535898384862238508 ) ) ;
#10041 = VERTEX_POINT ( 'NONE', #16877 ) ;
#10042 = LINE ( 'NONE', #16193, #3977 ) ;
#10043 = CARTESIAN_POINT ( 'NONE',  ( 3.469446951953614189E-15, 40.00000000000000000, 8.999999999999992895 ) ) ;
#10045 = ORIENTED_EDGE ( 'NONE', *, *, #20352, .F. ) ;
#10044 = CARTESIAN_POINT ( 'NONE',  ( 21.21320343559646915, 21.21320343559638744, 8.999999999999992895 ) ) ;
#10046 = EDGE_CURVE ( 'NONE', #4583, #7760, #8812, .T. ) ;
#10047 = AXIS2_PLACEMENT_3D ( 'NONE', #19702, #2182, #3882 ) ;
#10048 = VERTEX_POINT ( 'NONE', #18686 ) ;
#10049 = VERTEX_POINT ( 'NONE', #4712 ) ;
#10050 = PRODUCT ( 'MAS-166', 'MAS-166', '', ( #17754 ) ) ;
#10051 = ORIENTED_EDGE ( 'NONE', *, *, #22674, .F. ) ;
#10052 = CARTESIAN_POINT ( 'NONE',  ( 29.41953157733086854, -10.08469938919509801, -2.750000000000000000 ) ) ;
#10053 = DIRECTION ( 'NONE',  ( 0.000000000000000000, 0.000000000000000000, 1.000000000000000000 ) ) ;
#10054 = SURFACE_STYLE_FILL_AREA ( #2347 ) ;
#10055 = AXIS2_PLACEMENT_3D ( 'NONE', #19027, #4905, #729 ) ;
#10056 = CARTESIAN_POINT ( 'NONE',  ( 3.756430356250002323, 26.45312499938549067, 11.16877607737301226 ) ) ;
#10057 = CARTESIAN_POINT ( 'NONE',  ( -30.12293631110035363, 7.734255490827311341, 1.000000000000000000 ) ) ;
#10058 = CARTESIAN_POINT ( 'NONE',  ( 4.000000000000001776, -11.30940107675849760, 4.856249998770966414 ) ) ;
#10059 = FILL_AREA_STYLE_COLOUR ( '', #25618 ) ;
#10060 =( BOUNDED_SURFACE ( )  B_SPLINE_SURFACE ( 1, 2, ( 
 ( #10181, #6262, #22472, #12403, #12146, #765, #10568, #20511, #386, #8356, #24556, #10432, #14252, #22222, #525, #22613, #16480, #4308, #10692, #12281, #18565, #8738, #4552, #6644, #24048, #2346, #6130, #14116, #22079, #20122, #20247, #16345, #24312, #6397, #14387, #22345, #11203, #13310, #13064, #19325, #21043, #6909, #10818, #21283, #3118, #3365, #11083, #9265, #19064, #1147, #24699, #4822, #25085, #16986, #5328, #11342, #1419, #23245, #16725, #6785, #14770, #19183, #24950, #7030, #22746, #16867, #12926, #1280, #2991, #13189, #12799, #4941, #15018, #20773, #3232, #2851, #18812, #24833, #902, #9007, #17253, #21159, #9119, #17110, #8884, #7173, #14891, #22865, #25221, #20902, #10961, #18947, #7301, #15161, #22998, #1031, #5084, #23129, #5212, #15280, #11591, #13827, #15920, #17624, #11729, #11474, #21540, #15782, #3748, #17372, #15397, #11975, #21804, #23751, #3621, #19564, #11859, #5710, #1538, #19444, #15666 ),
 ( #1668, #9392, #25339, #13453, #19827, #7803, #21421, #9642, #5594, #13574, #19705, #23507, #7417, #9507, #1806, #3502, #21929, #23374, #9774, #17487, #9890, #5459, #25461, #17750, #7547, #13689, #23895, #25598, #23633, #15541, #7681, #21663, #25722, #5840, #3885, #1928, #17876, #25847, #7933, #5976, #13958, #4009, #19947, #12109, #22437, #20085, #6362, #6098, #2566, #22314, #14352, #20213, #24016, #18262, #22576, #2313, #4130, #22046, #6486, #101, #2428, #14472, #12493, #4515, #18390, #20469, #18013, #4392, #6606, #12372, #10390, #2187, #618, #14081, #10148, #8074, #10268, #18152, #16053, #224, #10534, #14592, #20336, #8195, #18532, #16171, #488, #24136, #6221, #16446, #8584, #8459, #16564, #24524, #8318, #14213, #12638, #4656, #2050, #22186, #24411, #10017, #4273, #12244, #348, #16306, #24274, #19152, #11169, #25047, #15123, #18772, #5045, #22711, #13027, #23212, #5296, #21122, #10779, #4792, #9227 ) ),
 .UNSPECIFIED., .F., .F., .F. ) 
 B_SPLINE_SURFACE_WITH_KNOTS ( ( 2, 2 ),
 ( 3, 2, 2, 2, 2, 2, 2, 2, 2, 2, 2, 2, 2, 2, 2, 2, 2, 2, 2, 2, 2, 2, 2, 2, 2, 2, 2, 2, 2, 2, 2, 2, 2, 2, 2, 2, 2, 2, 2, 2, 2, 2, 2, 2, 2, 2, 2, 2, 2, 2, 2, 2, 2, 2, 2, 2, 2, 2, 2, 2, 3 ),
 ( 0.000000000000000000, 1.000000000000000000 ),
 ( 0.000000000000000000, 0.01666666666666666644, 0.03333333333333333287, 0.05000000000000000278, 0.06666666666666666574, 0.08333333333333332871, 0.1000000000000000056, 0.1166666666666666685, 0.1333333333333333315, 0.1499999999999999944, 0.1666666666666666574, 0.1833333333333333204, 0.2000000000000000111, 0.2166666666666666741, 0.2333333333333333370, 0.2500000000000000000, 0.2666666666666666630, 0.2833333333333333259, 0.2999999999999999889, 0.3166666666666666519, 0.3333333333333333148, 0.3499999999999999778, 0.3666666666666666408, 0.3833333333333333592, 0.4000000000000000222, 0.4166666666666666852, 0.4333333333333333481, 0.4500000000000000111, 0.4666666666666666741, 0.4833333333333333370, 0.5000000000000000000, 0.5166666666666667185, 0.5333333333333333259, 0.5500000000000000444, 0.5666666666666666519, 0.5833333333333333703, 0.5999999999999999778, 0.6166666666666666963, 0.6333333333333333037, 0.6500000000000000222, 0.6666666666666666297, 0.6833333333333333481, 0.6999999999999999556, 0.7166666666666666741, 0.7333333333333332815, 0.7500000000000000000, 0.7666666666666667185, 0.7833333333333333259, 0.8000000000000000444, 0.8166666666666666519, 0.8333333333333333703, 0.8499999999999999778, 0.8666666666666666963, 0.8833333333333333037, 0.9000000000000000222, 0.9166666666666666297, 0.9333333333333333481, 0.9499999999999999556, 0.9666666666666666741, 0.9833333333333332815, 1.000000000000000000 ),
 .UNSPECIFIED. ) 
 GEOMETRIC_REPRESENTATION_ITEM ( )  RATIONAL_B_SPLINE_SURFACE ( (
 ( 1.000000000000000000, 0.8660254037844387076, 1.000000000000000000, 0.8660254037844387076, 1.000000000000000000, 0.8660254037844387076, 1.000000000000000000, 0.8660254037844387076, 1.000000000000000000, 0.8660254037844387076, 1.000000000000000000, 0.8660254037844387076, 1.000000000000000000, 0.8660254037844387076, 1.000000000000000000, 0.8660254037844387076, 1.000000000000000000, 0.8660254037844387076, 1.000000000000000000, 0.8660254037844387076, 1.000000000000000000, 0.8660254037844387076, 1.000000000000000000, 0.8660254037844387076, 1.000000000000000000, 0.8660254037844387076, 1.000000000000000000, 0.8660254037844387076, 1.000000000000000000, 0.8660254037844387076, 1.000000000000000000, 0.8660254037844387076, 1.000000000000000000, 0.8660254037844387076, 1.000000000000000000, 0.8660254037844387076, 1.000000000000000000, 0.8660254037844387076, 1.000000000000000000, 0.8660254037844387076, 1.000000000000000000, 0.8660254037844387076, 1.000000000000000000, 0.8660254037844387076, 1.000000000000000000, 0.8660254037844387076, 1.000000000000000000, 0.8660254037844387076, 1.000000000000000000, 0.8660254037844387076, 1.000000000000000000, 0.8660254037844387076, 1.000000000000000000, 0.8660254037844387076, 1.000000000000000000, 0.8660254037844387076, 1.000000000000000000, 0.8660254037844387076, 1.000000000000000000, 0.8660254037844387076, 1.000000000000000000, 0.8660254037844387076, 1.000000000000000000, 0.8660254037844387076, 1.000000000000000000, 0.8660254037844387076, 1.000000000000000000, 0.8660254037844387076, 1.000000000000000000, 0.8660254037844387076, 1.000000000000000000, 0.8660254037844387076, 1.000000000000000000, 0.8660254037844387076, 1.000000000000000000, 0.8660254037844387076, 1.000000000000000000, 0.8660254037844387076, 1.000000000000000000, 0.8660254037844387076, 1.000000000000000000, 0.8660254037844387076, 1.000000000000000000, 0.8660254037844387076, 1.000000000000000000, 0.8660254037844387076, 1.000000000000000000, 0.8660254037844387076, 1.000000000000000000, 0.8660254037844387076, 1.000000000000000000, 0.8660254037844387076, 1.000000000000000000, 0.8660254037844387076, 1.000000000000000000, 0.8660254037844387076, 1.000000000000000000, 0.8660254037844387076, 1.000000000000000000, 0.8660254037844387076, 1.000000000000000000, 0.8660254037844387076, 1.000000000000000000, 0.8660254037844387076, 1.000000000000000000, 0.8660254037844387076, 1.000000000000000000, 0.8660254037844387076, 1.000000000000000000, 0.8660254037844387076, 1.000000000000000000, 0.8660254037844387076, 1.000000000000000000, 0.8660254037844387076, 1.000000000000000000, 0.8660254037844387076, 1.000000000000000000, 0.8660254037844387076, 1.000000000000000000, 0.8660254037844387076, 1.000000000000000000),
 ( 1.000000000000000000, 0.8660254037844387076, 1.000000000000000000, 0.8660254037844387076, 1.000000000000000000, 0.8660254037844387076, 1.000000000000000000, 0.8660254037844387076, 1.000000000000000000, 0.8660254037844387076, 1.000000000000000000, 0.8660254037844387076, 1.000000000000000000, 0.8660254037844387076, 1.000000000000000000, 0.8660254037844387076, 1.000000000000000000, 0.8660254037844387076, 1.000000000000000000, 0.8660254037844387076, 1.000000000000000000, 0.8660254037844387076, 1.000000000000000000, 0.8660254037844387076, 1.000000000000000000, 0.8660254037844387076, 1.000000000000000000, 0.8660254037844387076, 1.000000000000000000, 0.8660254037844387076, 1.000000000000000000, 0.8660254037844387076, 1.000000000000000000, 0.8660254037844387076, 1.000000000000000000, 0.8660254037844387076, 1.000000000000000000, 0.8660254037844387076, 1.000000000000000000, 0.8660254037844387076, 1.000000000000000000, 0.8660254037844387076, 1.000000000000000000, 0.8660254037844387076, 1.000000000000000000, 0.8660254037844387076, 1.000000000000000000, 0.8660254037844387076, 1.000000000000000000, 0.8660254037844387076, 1.000000000000000000, 0.8660254037844387076, 1.000000000000000000, 0.8660254037844387076, 1.000000000000000000, 0.8660254037844387076, 1.000000000000000000, 0.8660254037844387076, 1.000000000000000000, 0.8660254037844387076, 1.000000000000000000, 0.8660254037844387076, 1.000000000000000000, 0.8660254037844387076, 1.000000000000000000, 0.8660254037844387076, 1.000000000000000000, 0.8660254037844387076, 1.000000000000000000, 0.8660254037844387076, 1.000000000000000000, 0.8660254037844387076, 1.000000000000000000, 0.8660254037844387076, 1.000000000000000000, 0.8660254037844387076, 1.000000000000000000, 0.8660254037844387076, 1.000000000000000000, 0.8660254037844387076, 1.000000000000000000, 0.8660254037844387076, 1.000000000000000000, 0.8660254037844387076, 1.000000000000000000, 0.8660254037844387076, 1.000000000000000000, 0.8660254037844387076, 1.000000000000000000, 0.8660254037844387076, 1.000000000000000000, 0.8660254037844387076, 1.000000000000000000, 0.8660254037844387076, 1.000000000000000000, 0.8660254037844387076, 1.000000000000000000, 0.8660254037844387076, 1.000000000000000000, 0.8660254037844387076, 1.000000000000000000, 0.8660254037844387076, 1.000000000000000000, 0.8660254037844387076, 1.000000000000000000, 0.8660254037844387076, 1.000000000000000000, 0.8660254037844387076, 1.000000000000000000, 0.8660254037844387076, 1.000000000000000000, 0.8660254037844387076, 1.000000000000000000, 0.8660254037844387076, 1.000000000000000000, 0.8660254037844387076, 1.000000000000000000, 0.8660254037844387076, 1.000000000000000000, 0.8660254037844387076, 1.000000000000000000) ) ) 
 REPRESENTATION_ITEM ( '' )  SURFACE ( )  );
#10061 = CARTESIAN_POINT ( 'NONE',  ( 1.878215178125004048, 26.11562499938548498, 5.746835883940462963 ) ) ;
#10062 = CARTESIAN_POINT ( 'NONE',  ( 0.000000000000000000, 0.000000000000000000, -6.500000000000000000 ) ) ;
#10063 = VECTOR ( 'NONE', #10756, 1000.000000000000000 ) ;
#10064 = CARTESIAN_POINT ( 'NONE',  ( 4.000000000000003553, 29.50000000000000355, 8.999999999999992895 ) ) ;
#10065 = CARTESIAN_POINT ( 'NONE',  ( 3.756430356250002323, 25.55312499938548498, 11.16877607737301403 ) ) ;
#10066 = DIRECTION ( 'NONE',  ( 1.000000000000000000, 0.000000000000000000, 0.000000000000000000 ) ) ;
#10067 = DIRECTION ( 'NONE',  ( 0.000000000000000000, 0.000000000000000000, -1.000000000000000000 ) ) ;
#10068 = CARTESIAN_POINT ( 'NONE',  ( -2.620986760973688460E-15, -28.43124999877096926, 13.61880215351699874 ) ) ;
#10069 = AXIS2_PLACEMENT_3D ( 'NONE', #19303, #13172, #21022 ) ;
#10070 = CARTESIAN_POINT ( 'NONE',  ( 3.735045420075836212E-15, 28.51562499938549067, 4.662447845253954171 ) ) ;
#10071 = CIRCLE ( 'NONE', #19259, 27.10000000000000142 ) ;
#10072 = CARTESIAN_POINT ( 'NONE',  ( 3.999999999999997335, -26.16250000000000142, 11.30940107675849404 ) ) ;
#10073 = CARTESIAN_POINT ( 'NONE',  ( 4.000000000000002665, 28.13124999877096855, 6.690598923241489970 ) ) ;
#10074 = CYLINDRICAL_SURFACE ( 'NONE', #18491, 0.5000000000000004441 ) ;
#10075 = VERTEX_POINT ( 'NONE', #534 ) ;
#10076 = CARTESIAN_POINT ( 'NONE',  ( -3.999999999999994671, 26.98750000000000426, 6.690598923241487306 ) ) ;
#10078 = ORIENTED_EDGE ( 'NONE', *, *, #3191, .T. ) ;
#10077 = CARTESIAN_POINT ( 'NONE',  ( -12.74173596767339767, 28.14012133169338270, -6.500000000000000000 ) ) ;
#10079 = VERTEX_POINT ( 'NONE', #8749 ) ;
#10080 = CARTESIAN_POINT ( 'NONE',  ( 3.469446951953614189E-15, -8.999999999999992895, 18.00000000000000000 ) ) ;
#10081 = EDGE_LOOP ( 'NONE', ( #52, #7261, #19853, #23152 ) ) ;
#10082 = ORIENTED_EDGE ( 'NONE', *, *, #576, .F. ) ;
#10083 = ORIENTED_EDGE ( 'NONE', *, *, #9367, .T. ) ;
#10084 = CARTESIAN_POINT ( 'NONE',  ( 22.75999951944203303, 17.10314526994957518, 6.690598923241489970 ) ) ;
#10085 = CIRCLE ( 'NONE', #6336, 0.5000000000000000000 ) ;
#10086 = ORIENTED_EDGE ( 'NONE', *, *, #12424, .F. ) ;
#10087 = CARTESIAN_POINT ( 'NONE',  ( -3.999999999999996003, 29.23750000000000071, 6.690598923241487306 ) ) ;
#10088 = CARTESIAN_POINT ( 'NONE',  ( -1.878215178124995832, 26.75312499938548783, 5.746835883940462963 ) ) ;
#10089 = VECTOR ( 'NONE', #4346, 1000.000000000000000 ) ;
#10090 = CARTESIAN_POINT ( 'NONE',  ( -3.756430356249996994, -8.999999999999992895, 0.4781249993854840286 ) ) ;
#10091 = DIRECTION ( 'NONE',  ( 0.000000000000000000, 0.000000000000000000, 1.000000000000000000 ) ) ;
#10092 = CARTESIAN_POINT ( 'NONE',  ( 18.81125008781888042, 18.81125008781880581, 4.662447845253954171 ) ) ;
#10093 = CIRCLE ( 'NONE', #18052, 0.5000000000000000000 ) ;
#10094 = FACE_OUTER_BOUND ( 'NONE', #18223, .T. ) ;
#10095 = FACE_OUTER_BOUND ( 'NONE', #9533, .T. ) ;
#10096 = ITEM_DEFINED_TRANSFORMATION ( 'NONE', 'NONE', #15651,  #21036 ) ;
#10097 = CARTESIAN_POINT ( 'NONE',  ( 1.878215178125004048, -5.746835883940462963, 1.115624999385483207 ) ) ;
#10098 = EDGE_CURVE ( 'NONE', #22312, #21505, #5058, .T. ) ;
#10099 = CARTESIAN_POINT ( 'NONE',  ( -1.999999999999998224, 28.90000000000000213, 12.46410161513774639 ) ) ;
#10100 = CARTESIAN_POINT ( 'NONE',  ( -3.756430356249997438, 28.10312499938548569, 11.16877607737301048 ) ) ;
#10101 = CARTESIAN_POINT ( 'NONE',  ( 23.65168074169088186, 18.16705623898524280, 8.999999999999992895 ) ) ;
#10102 = CARTESIAN_POINT ( 'NONE',  ( 21.99550407741325486, 19.33930669945380743, 12.25316411605952283 ) ) ;
#10103 = CARTESIAN_POINT ( 'NONE',  ( 4.000000000000003553, 28.15000000000000924, 8.999999999999992895 ) ) ;
#10104 = VERTEX_POINT ( 'NONE', #6795 ) ;
#10105 = ORIENTED_EDGE ( 'NONE', *, *, #11393, .T. ) ;
#10106 = CARTESIAN_POINT ( 'NONE',  ( 0.000000000000000000, 29.33124999877097139, 13.61880215351699874 ) ) ;
#10107 = VECTOR ( 'NONE', #16356, 1000.000000000000000 ) ;
#10108 = VECTOR ( 'NONE', #7185, 999.9999999999998863 ) ;
#10109 = EDGE_CURVE ( 'NONE', #11133, #1139, #9013, .T. ) ;
#10110 = ORIENTED_EDGE ( 'NONE', *, *, #3092, .F. ) ;
#10111 = DIRECTION ( 'NONE',  ( 0.000000000000000000, 0.000000000000000000, 1.000000000000000000 ) ) ;
#10112 = CARTESIAN_POINT ( 'NONE',  ( 1.878215178125004048, 25.77812499938548640, 5.746835883940462963 ) ) ;
#10113 = CARTESIAN_POINT ( 'NONE',  ( -1.022599059854450137E-14, 29.16250000000000497, 4.999999999999992006 ) ) ;
#10114 = VECTOR ( 'NONE', #3201, 1000.000000000000000 ) ;
#10115 = CARTESIAN_POINT ( 'NONE',  ( 4.648177544792955347E-16, 28.48750000000000071, 12.99999999999999289 ) ) ;
#10116 = EDGE_CURVE ( 'NONE', #4330, #7795, #13445, .T. ) ;
#10117 = VERTEX_POINT ( 'NONE', #2474 ) ;
#10118 = CIRCLE ( 'NONE', #4700, 0.5000000000000002220 ) ;
#10119 = DIRECTION ( 'NONE',  ( 0.000000000000000000, 1.000000000000000000, 0.000000000000000000 ) ) ;
#10120 = ORIENTED_EDGE ( 'NONE', *, *, #19273, .T. ) ;
#10121 = EDGE_CURVE ( 'NONE', #9415, #1627, #8381, .T. ) ;
#10122 = CARTESIAN_POINT ( 'NONE',  ( -27.10000000000000497, -0.5999999999999998668, 19.59999999999999787 ) ) ;
#10123 = CARTESIAN_POINT ( 'NONE',  ( 1.878215178125000939, 26.86562499938548498, 12.25316411605952283 ) ) ;
#10124 = CARTESIAN_POINT ( 'NONE',  ( 1.878215178125003382, 29.56562499938549138, 12.25316411605952283 ) ) ;
#10125 = CARTESIAN_POINT ( 'NONE',  ( -4.000000000000003553, -26.80000000000000071, 8.999999999999992895 ) ) ;
#10126 = CARTESIAN_POINT ( 'NONE',  ( -3.137519842735244810E-15, 26.46249999999999858, 4.999999999999991118 ) ) ;
#10127 = CARTESIAN_POINT ( 'NONE',  ( 3.347751660414011177, 29.81285215011482137, 11.20140010723572388 ) ) ;
#10128 = AXIS2_PLACEMENT_3D ( 'NONE', #6028, #6284, #20666 ) ;
#10129 = LINE ( 'NONE', #8174, #20974 ) ;
#10130 = CARTESIAN_POINT ( 'NONE',  ( 27.49048467073858859, 14.54246377227349463, -2.750000000000000000 ) ) ;
#10131 = CYLINDRICAL_SURFACE ( 'NONE', #6380, 0.5000000000000004441 ) ;
#10132 = CARTESIAN_POINT ( 'NONE',  ( -23.46296185032681336, 19.82388608118453632, 1.000000000000000000 ) ) ;
#10133 = CARTESIAN_POINT ( 'NONE',  ( -3.756430356250002323, -25.55312499938548498, 11.16877607737301403 ) ) ;
#10134 = VECTOR ( 'NONE', #14561, 1000.000000000000000 ) ;
#10135 = CARTESIAN_POINT ( 'NONE',  ( 4.000000000000003553, -8.999999999999992895, 18.00000000000000000 ) ) ;
#10136 = ORIENTED_EDGE ( 'NONE', *, *, #15699, .T. ) ;
#10137 = CARTESIAN_POINT ( 'NONE',  ( 3.752267015613588906E-15, 28.65624999877096712, 4.381197846482986158 ) ) ;
#10138 = CARTESIAN_POINT ( 'NONE',  ( -2.620986760973688460E-15, -28.48750000000000071, 13.61880215351699874 ) ) ;
#10140 = ORIENTED_EDGE ( 'NONE', *, *, #24866, .F. ) ;
#10139 = CARTESIAN_POINT ( 'NONE',  ( -3.756430356249994773, 26.37812499938548783, 8.999999999999992895 ) ) ;
#10141 = CARTESIAN_POINT ( 'NONE',  ( 2.672651547586948120E-15, 28.29062499938548925, 13.33755215474603162 ) ) ;
#10142 = CARTESIAN_POINT ( 'NONE',  ( 3.918623196469464443, 38.49999999999999289, 4.456389954662531849 ) ) ;
#10143 = CARTESIAN_POINT ( 'NONE',  ( 1.071796769724492338, 26.20134618820330275, 12.99999999999999467 ) ) ;
#10144 = ORIENTED_EDGE ( 'NONE', *, *, #2940, .T. ) ;
#10145 = ORIENTED_EDGE ( 'NONE', *, *, #20012, .F. ) ;
#10146 = EDGE_CURVE ( 'NONE', #20673, #24553, #9513, .T. ) ;
#10147 = SURFACE_SIDE_STYLE ('',( #1667 ) ) ;
#10148 = CARTESIAN_POINT ( 'NONE',  ( 1.878215178125006934, 27.91562499938549280, 5.746835883940462963 ) ) ;
#10149 = CARTESIAN_POINT ( 'NONE',  ( -4.000000000000003553, -28.99374999877096926, 8.999999999999992895 ) ) ;
#10150 = EDGE_CURVE ( 'NONE', #13852, #9588, #24700, .T. ) ;
#10151 = AXIS2_PLACEMENT_3D ( 'NONE', #11144, #12998, #19007 ) ;
#10152 = CARTESIAN_POINT ( 'NONE',  ( -3.756430356249996105, -6.831223922626973533, 3.028124999385485072 ) ) ;
#10153 = EDGE_CURVE ( 'NONE', #22773, #9061, #1291, .T. ) ;
#10154 = AXIS2_PLACEMENT_3D ( 'NONE', #24797, #2569, #14737 ) ;
#10155 = CARTESIAN_POINT ( 'NONE',  ( 30.85476721088027929, 3.897863563849760737, 1.000000000000000000 ) ) ;
#10156 = CYLINDRICAL_SURFACE ( 'NONE', #13770, 0.5000000000000004441 ) ;
#10157 = DIRECTION ( 'NONE',  ( -0.000000000000000000, -1.000000000000000000, -0.000000000000000000 ) ) ;
#10158 = DIRECTION ( 'NONE',  ( 0.000000000000000000, -0.000000000000000000, 1.000000000000000000 ) ) ;
#10159 = ADVANCED_FACE ( 'NONE', ( #21547 ), #17495, .F. ) ;
#10160 = CARTESIAN_POINT ( 'NONE',  ( 11.91206721063030649, -28.72825533807137433, 1.000000000000000000 ) ) ;
#10161 = CARTESIAN_POINT ( 'NONE',  ( -3.999999999999996447, 26.48124999877096997, 6.690598923241487306 ) ) ;
#10162 = CARTESIAN_POINT ( 'NONE',  ( 20.72498534553237093, 15.41259058961355954, 11.16877607737301226 ) ) ;
#10163 = CARTESIAN_POINT ( 'NONE',  ( 17.22246953840583217, 22.87932378789814436, 11.30940107675849404 ) ) ;
#10164 = VERTEX_POINT ( 'NONE', #21296 ) ;
#10165 = DIRECTION ( 'NONE',  ( 0.000000000000000000, 0.000000000000000000, 1.000000000000000000 ) ) ;
#10166 = DIRECTION ( 'NONE',  ( 0.000000000000000000, 0.000000000000000000, 1.000000000000000000 ) ) ;
#10167 = CARTESIAN_POINT ( 'NONE',  ( 1.878215178125004048, 25.66562499938548569, 5.746835883940462963 ) ) ;
#10168 = CARTESIAN_POINT ( 'NONE',  ( -0.2646063747045178660, 30.00000000000000000, 4.999999999999992895 ) ) ;
#10169 = DIRECTION ( 'NONE',  ( 0.9297764858882504591, -0.3681245526846803617, 0.000000000000000000 ) ) ;
#10170 = ORIENTED_EDGE ( 'NONE', *, *, #16798, .T. ) ;
#10171 = FACE_OUTER_BOUND ( 'NONE', #7251, .T. ) ;
#10172 = CARTESIAN_POINT ( 'NONE',  ( -1.999999999999995781, 26.44374999877096855, 5.535898384862237620 ) ) ;
#10173 = CARTESIAN_POINT ( 'NONE',  ( -3.756430356250002323, -26.45312499938548356, 11.16877607737301226 ) ) ;
#10175 = ORIENTED_EDGE ( 'NONE', *, *, #8740, .F. ) ;
#10174 = DIRECTION ( 'NONE',  ( 0.000000000000000000, 0.000000000000000000, 1.000000000000000000 ) ) ;
#10176 = ORIENTED_EDGE ( 'NONE', *, *, #15604, .T. ) ;
#10177 = ADVANCED_FACE ( 'NONE', ( #3629 ), #21429, .F. ) ;
#10178 = ORIENTED_EDGE ( 'NONE', *, *, #17270, .F. ) ;
#10179 = ORIENTED_EDGE ( 'NONE', *, *, #24020, .F. ) ;
#10180 = DIRECTION ( 'NONE',  ( 0.000000000000000000, 0.000000000000000000, 1.000000000000000000 ) ) ;
#10181 = CARTESIAN_POINT ( 'NONE',  ( 3.756430356250004987, 25.25312499938548427, 8.999999999999992895 ) ) ;
#10182 = ADVANCED_FACE ( 'NONE', ( #9397 ), #1153, .F. ) ;
#10183 = CARTESIAN_POINT ( 'NONE',  ( 3.756430356250006319, 26.97812499938548569, 6.831223922626973533 ) ) ;
#10184 = DIRECTION ( 'NONE',  ( 0.000000000000000000, 0.000000000000000000, 1.000000000000000000 ) ) ;
#10185 = CARTESIAN_POINT ( 'NONE',  ( 3.752267015613588906E-15, -4.381197846482986158, 3.206249998770963838 ) ) ;
#10186 =( NAMED_UNIT ( * ) PLANE_ANGLE_UNIT ( ) SI_UNIT ( $, .RADIAN. ) );
#10187 = CARTESIAN_POINT ( 'NONE',  ( -1.878215178124995832, 25.74062499938548498, 5.746835883940462963 ) ) ;
#10188 = ADVANCED_FACE ( 'NONE', ( #7560 ), #5602, .F. ) ;
#10189 = DIRECTION ( 'NONE',  ( -0.000000000000000000, -1.000000000000000000, -0.000000000000000000 ) ) ;
#10190 = CARTESIAN_POINT ( 'NONE',  ( 2.000000000000000888, -12.46410161513774817, 1.668749998770965970 ) ) ;
#10191 = CARTESIAN_POINT ( 'NONE',  ( 1.878215178125000939, 26.41562499938548214, 12.25316411605952283 ) ) ;
#10192 = DIRECTION ( 'NONE',  ( 1.000000000000000000, 0.000000000000000000, 0.000000000000000000 ) ) ;
#10193 = PLANE ( 'NONE',  #14547 ) ;
#10194 = CARTESIAN_POINT ( 'NONE',  ( 15.30002297792396071, 20.95687722741627468, 6.690598923241487306 ) ) ;
#10195 = CARTESIAN_POINT ( 'NONE',  ( 3.756430356249997882, -25.51562499938548356, 11.16877607737301226 ) ) ;
#10196 = DIRECTION ( 'NONE',  ( 0.000000000000000000, 0.000000000000000000, 1.000000000000000000 ) ) ;
#10197 = CARTESIAN_POINT ( 'NONE',  ( 3.999999999999995559, -26.08749999999999503, 6.690598923241487306 ) ) ;
#10198 = CARTESIAN_POINT ( 'NONE',  ( 3.794751686895379894, -29.75919970560060079, 7.708599238039753665 ) ) ;
#10199 = ORIENTED_EDGE ( 'NONE', *, *, #3452, .T. ) ;
#10200 = CARTESIAN_POINT ( 'NONE',  ( 4.000000000000001776, 28.56249999999999645, 11.30940107675849760 ) ) ;
#10202 = ORIENTED_EDGE ( 'NONE', *, *, #12366, .F. ) ;
#10201 = CARTESIAN_POINT ( 'NONE',  ( -0.7500000000000000000, -1.299038105676658450, 17.69999999999999929 ) ) ;
#10203 = ORIENTED_EDGE ( 'NONE', *, *, #11555, .F. ) ;
#10204 = ORIENTED_EDGE ( 'NONE', *, *, #15730, .T. ) ;
#10205 = ORIENTED_EDGE ( 'NONE', *, *, #25395, .F. ) ;
#10206 = VERTEX_POINT ( 'NONE', #25094 ) ;
#10207 = CARTESIAN_POINT ( 'NONE',  ( 5.840899737312979845, 38.49999999999999289, 10.37254881831474052 ) ) ;
#10208 = ORIENTED_EDGE ( 'NONE', *, *, #17759, .T. ) ;
#10209 = DIRECTION ( 'NONE',  ( -0.000000000000000000, -1.000000000000000000, -0.000000000000000000 ) ) ;
#10210 = CARTESIAN_POINT ( 'NONE',  ( 3.735045420075836212E-15, 26.71562499938548285, 4.662447845253954171 ) ) ;
#10211 =( BOUNDED_CURVE ( )  B_SPLINE_CURVE ( 2, ( #21621, #7505, #15878, #11685, #5674, #9856, #19407, #21892, #19660 ),
 .UNSPECIFIED., .F., .F. ) 
 B_SPLINE_CURVE_WITH_KNOTS ( ( 3, 2, 2, 2, 3 ),
 ( 0.5750000000000000666, 0.5833333333333333703, 0.5999999999999999778, 0.6166666666666666963, 0.6250000000000000000 ),
 .UNSPECIFIED. ) 
 CURVE ( )  GEOMETRIC_REPRESENTATION_ITEM ( )  RATIONAL_B_SPLINE_CURVE ( ( 0.9330127018922194093, 0.9330127018922198534, 1.000000000000000000, 0.8660254037844387076, 1.000000000000000000, 0.8660254037844387076, 1.000000000000000000, 0.9330127018922194093, 0.9330127018922194093 ) ) 
 REPRESENTATION_ITEM ( '' )  );
#10212 = AXIS2_PLACEMENT_3D ( 'NONE', #1382, #5293, #15244 ) ;
#10213 = EDGE_CURVE ( 'NONE', #2722, #6155, #11213, .T. ) ;
#10214 = CARTESIAN_POINT ( 'NONE',  ( -3.756430356249995661, -6.831223922626973533, 2.240624999385484539 ) ) ;
#10215 = CARTESIAN_POINT ( 'NONE',  ( -13.24173596767398742, -28.14012133169310559, -6.500000000000000000 ) ) ;
#10216 = CARTESIAN_POINT ( 'NONE',  ( 18.57032807491351178, 21.22652545287281356, 12.25316411605951927 ) ) ;
#10217 = DIRECTION ( 'NONE',  ( 1.000000000000000000, 0.000000000000000000, 0.000000000000000000 ) ) ;
#10218 = CARTESIAN_POINT ( 'NONE',  ( 3.469446951953614189E-15, -8.999999999999992895, 18.00000000000000000 ) ) ;
#10219 = ITEM_DEFINED_TRANSFORMATION ( 'NONE', 'NONE', #9377,  #21036 ) ;
#10220 = CARTESIAN_POINT ( 'NONE',  ( 3.756430356250002323, -11.16877607737301226, 0.5531249993854806535 ) ) ;
#10221 = DIRECTION ( 'NONE',  ( 0.000000000000000000, 1.000000000000000000, 0.000000000000000000 ) ) ;
#10222 = CARTESIAN_POINT ( 'NONE',  ( 1.859271017917182139E-15, 28.93749999999999645, 12.99999999999999289 ) ) ;
#10223 = CARTESIAN_POINT ( 'NONE',  ( 3.469446951953614189E-15, 25.00000000000000000, 8.999999999999992895 ) ) ;
#10224 = DIRECTION ( 'NONE',  ( 1.000000000000000000, 0.000000000000000000, 0.000000000000000000 ) ) ;
#10225 = DIRECTION ( 'NONE',  ( -1.000000000000000000, 0.000000000000000000, 0.000000000000000000 ) ) ;
#10226 = VERTEX_POINT ( 'NONE', #23138 ) ;
#10227 = VERTEX_POINT ( 'NONE', #11599 ) ;
#10228 = CARTESIAN_POINT ( 'NONE',  ( 1.878215178124999829, 26.97812499938549280, 12.25316411605952283 ) ) ;
#10229 = ORIENTED_EDGE ( 'NONE', *, *, #18537, .F. ) ;
#10230 = CARTESIAN_POINT ( 'NONE',  ( 26.49999999999999645, 0.5000000000000000000, 19.50000000000000000 ) ) ;
#10231 = ORIENTED_EDGE ( 'NONE', *, *, #20484, .F. ) ;
#10232 = CARTESIAN_POINT ( 'NONE',  ( 19.95366948073886348, 17.12524235599260791, 12.46410161513774817 ) ) ;
#10233 = ORIENTED_EDGE ( 'NONE', *, *, #25420, .T. ) ;
#10234 = CIRCLE ( 'NONE', #21932, 3.000000000000000444 ) ;
#10235 = CARTESIAN_POINT ( 'NONE',  ( 31.06601413805602263, -1.453535542772716793, 1.000000000000000000 ) ) ;
#10236 = ORIENTED_EDGE ( 'NONE', *, *, #12394, .T. ) ;
#10237 = CARTESIAN_POINT ( 'NONE',  ( -7.234255490826573265, 30.12293631110053838, -6.500000000000000000 ) ) ;
#10238 = CARTESIAN_POINT ( 'NONE',  ( -1.878215178124998497, 27.24062499938548498, 12.25316411605951927 ) ) ;
#10239 = CARTESIAN_POINT ( 'NONE',  ( -3.756430356249997882, 29.41562499938548569, 8.999999999999992895 ) ) ;
#10240 = EDGE_CURVE ( 'NONE', #18460, #5942, #15169, .T. ) ;
#10241 = CARTESIAN_POINT ( 'NONE',  ( 8.217531866530997320, -29.99470236596036088, -6.500000000000000000 ) ) ;
#10242 = CARTESIAN_POINT ( 'NONE',  ( 1.071796769724492338, 29.35134618820330488, 12.99999999999999467 ) ) ;
#10243 = CARTESIAN_POINT ( 'NONE',  ( 3.213722874945784014, 29.82775332956657266, 11.39306173506716924 ) ) ;
#10244 = ADVANCED_FACE ( 'NONE', ( #19195 ), #13073, .F. ) ;
#10245 = AXIS2_PLACEMENT_3D ( 'NONE', #20578, #25250, #2668 ) ;
#10246 = CARTESIAN_POINT ( 'NONE',  ( 3.756430356250003655, 25.59062499938548285, 8.999999999999992895 ) ) ;
#10247 = EDGE_CURVE ( 'NONE', #23781, #17588, #9672, .T. ) ;
#10248 = FACE_OUTER_BOUND ( 'NONE', #14469, .T. ) ;
#10249 = CARTESIAN_POINT ( 'NONE',  ( 17.52740933866159168, 23.18426358815389676, 6.690598923241487306 ) ) ;
#10250 = CARTESIAN_POINT ( 'NONE',  ( 21.28941499438225904, 22.67092431280586240, -6.500000000000000000 ) ) ;
#10251 = EDGE_CURVE ( 'NONE', #17688, #12485, #17636, .T. ) ;
#10252 = CARTESIAN_POINT ( 'NONE',  ( 3.752267015613588906E-15, -4.381197846482986158, 4.556249998770967480 ) ) ;
#10253 = CARTESIAN_POINT ( 'NONE',  ( 4.000000000000003553, 25.00000000000000000, 8.999999999999992895 ) ) ;
#10254 = CARTESIAN_POINT ( 'NONE',  ( 1.878215178124995832, -26.19062499938548427, 5.746835883940462963 ) ) ;
#10255 = CARTESIAN_POINT ( 'NONE',  ( -3.999999999999996447, -8.999999999999992895, 0.2249999999999995060 ) ) ;
#10256 = ORIENTED_EDGE ( 'NONE', *, *, #6314, .F. ) ;
#10257 = CARTESIAN_POINT ( 'NONE',  ( 4.000000000000001776, 28.05624999877096926, 11.30940107675849760 ) ) ;
#10258 = DIRECTION ( 'NONE',  ( -1.000000000000000000, 2.891205793294678326E-16, 0.000000000000000000 ) ) ;
#10260 = EDGE_LOOP ( 'NONE', ( #8548, #15384, #22956, #12749 ) ) ;
#10259 = CARTESIAN_POINT ( 'NONE',  ( 8.012344526598182026E-15, 28.06562499938548783, 4.662447845253954171 ) ) ;
#10261 = ORIENTED_EDGE ( 'NONE', *, *, #5399, .T. ) ;
#10262 = DIRECTION ( 'NONE',  ( 0.000000000000000000, 0.000000000000000000, 1.000000000000000000 ) ) ;
#10263 = CARTESIAN_POINT ( 'NONE',  ( 2.000000000000000000, 27.17500000000000426, 12.46410161513774817 ) ) ;
#10264 = DIRECTION ( 'NONE',  ( 0.000000000000000000, 0.000000000000000000, 1.000000000000000000 ) ) ;
#10265 = ORIENTED_EDGE ( 'NONE', *, *, #22721, .T. ) ;
#10266 = ORIENTED_EDGE ( 'NONE', *, *, #20012, .T. ) ;
#10267 = CARTESIAN_POINT ( 'NONE',  ( 1.878215178124998497, -26.90312499938548285, 12.25316411605951927 ) ) ;
#10268 = CARTESIAN_POINT ( 'NONE',  ( -1.878215178124994722, 27.99062499938548143, 5.746835883940462963 ) ) ;
#10269 = LINE ( 'NONE', #18391, #16389 ) ;
#10270 = CARTESIAN_POINT ( 'NONE',  ( -3.756430356249996105, -6.831223922626973533, 3.928124999385480542 ) ) ;
#10271 = EDGE_CURVE ( 'NONE', #6029, #15121, #25607, .T. ) ;
#10272 = DIRECTION ( 'NONE',  ( 0.000000000000000000, 0.000000000000000000, 1.000000000000000000 ) ) ;
#10273 = PRODUCT_DEFINITION ( 'UNKNOWN', '', #15226, #14902 ) ;
#10274 = CARTESIAN_POINT ( 'NONE',  ( 1.859271017917182139E-15, 29.33124999877096428, 12.99999999999999289 ) ) ;
#10275 =( BOUNDED_CURVE ( )  B_SPLINE_CURVE ( 2, ( #19306, #11842, #11457, #23735, #25443, #3869, #1403 ),
 .UNSPECIFIED., .F., .F. ) 
 B_SPLINE_CURVE_WITH_KNOTS ( ( 3, 2, 2, 3 ),
 ( 0.5499999999999997113, 0.5666666666666665408, 0.5833333333333335924, 0.6000000000000004219 ),
 .UNSPECIFIED. ) 
 CURVE ( )  GEOMETRIC_REPRESENTATION_ITEM ( )  RATIONAL_B_SPLINE_CURVE ( ( 1.000000000000002665, 0.8660254037844360431, 1.000000000000000000, 0.8660254037844387076, 1.000000000000000000, 0.8660254037844351549, 1.000000000000003553 ) ) 
 REPRESENTATION_ITEM ( '' )  );
#10276 = CARTESIAN_POINT ( 'NONE',  ( 20.58122674904192451, 20.58122674904186411, 4.999999999999992006 ) ) ;
#10277 = CARTESIAN_POINT ( 'NONE',  ( 20.62984034111755705, 17.80141321637130147, 12.46410161513774817 ) ) ;
#10278 = DIRECTION ( 'NONE',  ( 1.000000000000000000, 0.000000000000000000, 0.000000000000000000 ) ) ;
#10279 = CARTESIAN_POINT ( 'NONE',  ( 3.834746474454188013E-15, 25.56250000000000000, 4.999999999999992006 ) ) ;
#10280 = CARTESIAN_POINT ( 'NONE',  ( 18.65215106205190310, 18.65215106205183915, 13.33755215474602984 ) ) ;
#10281 = CARTESIAN_POINT ( 'NONE',  ( 21.33252770405263732, 18.50410057930636754, 5.535898384862238508 ) ) ;
#10282 = EDGE_CURVE ( 'NONE', #24763, #22773, #7146, .T. ) ;
#10283 = EDGE_LOOP ( 'NONE', ( #9640, #5004, #17834, #17430 ) ) ;
#10284 = CARTESIAN_POINT ( 'NONE',  ( 6.317933499823438659, 30.45149776762727356, -6.500000000000000000 ) ) ;
#10285 = CARTESIAN_POINT ( 'NONE',  ( 3.872397317694597163, 29.74907003676636563, 7.964378325765101962 ) ) ;
#10286 = CARTESIAN_POINT ( 'NONE',  ( 1.878215178125004048, 29.37812499938548783, 5.746835883940462963 ) ) ;
#10287 = ADVANCED_FACE ( 'NONE', ( #13320 ), #19333, .F. ) ;
#10289 = VERTEX_POINT ( 'NONE', #19455 ) ;
#10288 = CARTESIAN_POINT ( 'NONE',  ( -3.871726839561290490, 29.74915783848840434, 10.03836643961818886 ) ) ;
#10290 = CARTESIAN_POINT ( 'NONE',  ( 17.19146985159974150, 19.84766722955904683, 5.746835883940462963 ) ) ;
#10291 = CARTESIAN_POINT ( 'NONE',  ( 1.071796769724481901, -28.01740381056766438, 12.99999999999999645 ) ) ;
#10292 = ORIENTED_EDGE ( 'NONE', *, *, #6643, .F. ) ;
#10293 = CARTESIAN_POINT ( 'NONE',  ( 5.827558883616049457, 30.54913349766221842, -6.500000000000000000 ) ) ;
#10294 = CARTESIAN_POINT ( 'NONE',  ( -1.999999999999998224, 26.59374999877096712, 12.46410161513774639 ) ) ;
#10295 = CARTESIAN_POINT ( 'NONE',  ( -3.756430356250002323, -27.35312499938547859, 11.16877607737301226 ) ) ;
#10296 = ORIENTED_EDGE ( 'NONE', *, *, #13854, .T. ) ;
#10297 = EDGE_LOOP ( 'NONE', ( #1624, #6483, #22505, #14767 ) ) ;
#10298 = EDGE_LOOP ( 'NONE', ( #1731, #13405 ) ) ;
#10299 = ORIENTED_EDGE ( 'NONE', *, *, #2204, .T. ) ;
#10300 = DIRECTION ( 'NONE',  ( 0.000000000000000000, 0.000000000000000000, -1.000000000000000000 ) ) ;
#10301 = B_SPLINE_CURVE_WITH_KNOTS ( 'NONE', 3,
 ( #13929, #19799, #13791, #2016, #25424, #23471, #9984, #5560, #17977, #7647 ),
 .UNSPECIFIED., .F., .F.,
 ( 4, 2, 2, 2, 4 ),
 ( 2.789812635319129240E-07, 0.0002324414413947202324, 0.0004646039015259085148, 0.0006967663616570968785, 0.0009289288217882851880 ),
 .UNSPECIFIED. ) ;
#10302 = CARTESIAN_POINT ( 'NONE',  ( -3.137519842735244810E-15, 26.85624999877096641, 4.999999999999991118 ) ) ;
#10303 = CARTESIAN_POINT ( 'NONE',  ( -5.827558883615604479, 30.54913349766230724, 1.000000000000000000 ) ) ;
#10304 = CARTESIAN_POINT ( 'NONE',  ( 3.756430356250004099, -6.831223922626973533, 0.7406249993854815417 ) ) ;
#10305 = FILL_AREA_STYLE ('',( #12153 ) ) ;
#10306 = CARTESIAN_POINT ( 'NONE',  ( -3.756430356249995661, 27.12812499938548427, 6.831223922626973533 ) ) ;
#10307 = LINE ( 'NONE', #17794, #23006 ) ;
#10308 = DIRECTION ( 'NONE',  ( 1.000000000000000000, 0.000000000000000000, 0.000000000000000000 ) ) ;
#10309 = EDGE_CURVE ( 'NONE', #18698, #9952, #4142, .T. ) ;
#10310 = CARTESIAN_POINT ( 'NONE',  ( 3.756430356250003655, 27.39062499938548356, 8.999999999999992895 ) ) ;
#10311 = DIRECTION ( 'NONE',  ( 1.000000000000000000, 0.000000000000000000, 0.000000000000000000 ) ) ;
#10312 = DIRECTION ( 'NONE',  ( -1.000000000000000000, 0.000000000000000000, 0.000000000000000000 ) ) ;
#10313 = DIRECTION ( 'NONE',  ( 0.000000000000000000, 0.000000000000000000, 1.000000000000000000 ) ) ;
#10314 = CARTESIAN_POINT ( 'NONE',  ( 3.999999999999996447, -28.76874999877096784, 8.999999999999992895 ) ) ;
#10315 = LINE ( 'NONE', #20382, #13599 ) ;
#10316 = ADVANCED_FACE ( 'NONE', ( #16178 ), #5983, .F. ) ;
#10317 = CARTESIAN_POINT ( 'NONE',  ( 12.78762572734049030, -28.34936733434204470, 1.000000000000000000 ) ) ;
#10318 = CARTESIAN_POINT ( 'NONE',  ( -1.999999999999995781, 29.59374999877096712, 5.535898384862237620 ) ) ;
#10319 = CARTESIAN_POINT ( 'NONE',  ( -8.000000000000000000, 10.00000000000000178, 15.00000000000000178 ) ) ;
#10320 = VERTEX_POINT ( 'NONE', #2199 ) ;
#10321 = CYLINDRICAL_SURFACE ( 'NONE', #13768, 0.5000000000000004441 ) ;
#10323 = VERTEX_POINT ( 'NONE', #17758 ) ;
#10322 = CARTESIAN_POINT ( 'NONE',  ( -3.999999999999996447, -8.999999999999992895, 3.768749998770966947 ) ) ;
#10324 = VERTEX_POINT ( 'NONE', #19717 ) ;
#10325 = VERTEX_POINT ( 'NONE', #7944 ) ;
#10326 = ORIENTED_EDGE ( 'NONE', *, *, #21775, .F. ) ;
#10327 = VERTEX_POINT ( 'NONE', #7689 ) ;
#10328 = ORIENTED_EDGE ( 'NONE', *, *, #23515, .T. ) ;
#10329 = FACE_OUTER_BOUND ( 'NONE', #25268, .T. ) ;
#10330 = ORIENTED_EDGE ( 'NONE', *, *, #5087, .T. ) ;
#10331 = CARTESIAN_POINT ( 'NONE',  ( -3.999999999999996447, 28.82499999999999929, 8.999999999999992895 ) ) ;
#10332 = CARTESIAN_POINT ( 'NONE',  ( -3.756430356249996994, 26.37812499938548783, 8.999999999999992895 ) ) ;
#10333 = CARTESIAN_POINT ( 'NONE',  ( 3.756430356250003655, -8.999999999999992895, 3.403124999385484628 ) ) ;
#10334 = CARTESIAN_POINT ( 'NONE',  ( 5.112995299272250684E-15, 26.01250000000000284, 4.999999999999992006 ) ) ;
#10335 = CARTESIAN_POINT ( 'NONE',  ( 16.20808571844850121, 21.52048047436717937, 6.831223922626973533 ) ) ;
#10336 = LINE ( 'NONE', #18333, #13408 ) ;
#10337 = CARTESIAN_POINT ( 'NONE',  ( 3.735045420075836212E-15, -4.662447845253954171, 0.7031249993854805647 ) ) ;
#10338 = DIRECTION ( 'NONE',  ( 1.000000000000000000, 0.000000000000000000, 0.000000000000000000 ) ) ;
#10339 = EDGE_CURVE ( 'NONE', #7709, #6515, #24026, .T. ) ;
#10340 = CARTESIAN_POINT ( 'NONE',  ( -3.756430356249997438, 29.45312499938548356, 11.16877607737301048 ) ) ;
#10341 = CARTESIAN_POINT ( 'NONE',  ( -1.878215178124995832, -5.746835883940462963, 1.753124999385485827 ) ) ;
#10342 = CARTESIAN_POINT ( 'NONE',  ( 30.00000000000000355, 3.673940397442059967E-15, 20.00000000000000000 ) ) ;
#10343 = CYLINDRICAL_SURFACE ( 'NONE', #4094, 31.10000000000000142 ) ;
#10344 = ORIENTED_EDGE ( 'NONE', *, *, #20164, .T. ) ;
#10345 = ORIENTED_EDGE ( 'NONE', *, *, #2480, .F. ) ;
#10346 = CARTESIAN_POINT ( 'NONE',  ( 1.878215178125001605, 27.42812499938548854, 12.25316411605952283 ) ) ;
#10347 = ADVANCED_FACE ( 'NONE', ( #25856 ), #4016, .F. ) ;
#10348 = ORIENTED_EDGE ( 'NONE', *, *, #23410, .F. ) ;
#10349 = CARTESIAN_POINT ( 'NONE',  ( 0.4999838450258491940, 31.09598070739550124, 1.000000000000000000 ) ) ;
#10350 = ORIENTED_EDGE ( 'NONE', *, *, #3301, .F. ) ;
#10351 = CARTESIAN_POINT ( 'NONE',  ( -3.999999999999995559, 26.08749999999999503, 6.690598923241487306 ) ) ;
#10352 = ORIENTED_EDGE ( 'NONE', *, *, #670, .T. ) ;
#10353 = EDGE_CURVE ( 'NONE', #25487, #8252, #18431, .T. ) ;
#10354 = AXIS2_PLACEMENT_3D ( 'NONE', #10410, #4293, #24424 ) ;
#10355 = DIRECTION ( 'NONE',  ( 0.000000000000000000, 0.000000000000000000, 1.000000000000000000 ) ) ;
#10356 = ORIENTED_EDGE ( 'NONE', *, *, #19639, .F. ) ;
#10357 = CYLINDRICAL_SURFACE ( 'NONE', #23106, 4.000000000000000000 ) ;
#10358 = CARTESIAN_POINT ( 'NONE',  ( -1.878215178124998497, 26.79062499938548214, 12.25316411605951927 ) ) ;
#10359 = CARTESIAN_POINT ( 'NONE',  ( -14.54246377227330456, 27.49048467073868451, 1.000000000000000000 ) ) ;
#10360 = AXIS2_PLACEMENT_3D ( 'NONE', #14696, #12453, #701 ) ;
#10361 = AXIS2_PLACEMENT_3D ( 'NONE', #20848, #22818, #19240 ) ;
#10362 = CARTESIAN_POINT ( 'NONE',  ( 0.000000000000000000, 0.000000000000000000, 20.00000000000000000 ) ) ;
#10363 = DIRECTION ( 'NONE',  ( 0.000000000000000000, 0.000000000000000000, -1.000000000000000000 ) ) ;
#10364 = CARTESIAN_POINT ( 'NONE',  ( -3.999999999999996447, 28.78750000000000497, 6.690598923241487306 ) ) ;
#10365 = CARTESIAN_POINT ( 'NONE',  ( -3.756430356249995661, 28.02812499938548640, 6.831223922626973533 ) ) ;
#10366 = CARTESIAN_POINT ( 'NONE',  ( 20.53936981547090568, 15.22697505955208896, 6.831223922626973533 ) ) ;
#10367 = CIRCLE ( 'NONE', #17080, 0.5000000000000004441 ) ;
#10368 = VECTOR ( 'NONE', #25438, 1000.000000000000000 ) ;
#10369 = CARTESIAN_POINT ( 'NONE',  ( 22.22083059878729117, 19.39240347404102849, 12.46410161513774817 ) ) ;
#10370 = CARTESIAN_POINT ( 'NONE',  ( -0.5000000000000000000, -2.999999999999999556, 19.50000000000000000 ) ) ;
#10371 = CARTESIAN_POINT ( 'NONE',  ( 30.00000000000000355, 3.673940397442059967E-15, 20.00000000000000000 ) ) ;
#10373 = CARTESIAN_POINT ( 'NONE',  ( 3.756430356249997438, -25.40312499938548285, 11.16877607737301048 ) ) ;
#10372 = VECTOR ( 'NONE', #24790, 1000.000000000000000 ) ;
#10374 = ADVANCED_FACE ( 'NONE', ( #8205 ), #3759, .T. ) ;
#10375 = LINE ( 'NONE', #4378, #15020 ) ;
#10376 = VERTEX_POINT ( 'NONE', #11982 ) ;
#10377 = CARTESIAN_POINT ( 'NONE',  ( 3.752267015613588906E-15, 29.10624999877096997, 4.381197846482986158 ) ) ;
#10378 = CARTESIAN_POINT ( 'NONE',  ( 20.90826363534070254, 18.07983651059444696, 12.46410161513774817 ) ) ;
#10380 = ORIENTED_EDGE ( 'NONE', *, *, #2915, .T. ) ;
#10379 = CARTESIAN_POINT ( 'NONE',  ( 3.756430356250002323, 28.44062499938548783, 6.831223922626973533 ) ) ;
#10381 = ORIENTED_EDGE ( 'NONE', *, *, #20451, .T. ) ;
#10382 = CARTESIAN_POINT ( 'NONE',  ( 0.000000000000000000, 0.000000000000000000, 1.000000000000000000 ) ) ;
#10383 = EDGE_CURVE ( 'NONE', #24134, #9107, #1815, .T. ) ;
#10384 = CARTESIAN_POINT ( 'NONE',  ( -30.91344420362543843, 3.401318489841417048, -6.500000000000000000 ) ) ;
#10385 = CARTESIAN_POINT ( 'NONE',  ( -5.327558883615603591, 30.54913349766230724, -6.500000000000000000 ) ) ;
#10386 = EDGE_CURVE ( 'NONE', #9389, #16191, #9897, .T. ) ;
#10387 = EDGE_LOOP ( 'NONE', ( #16258, #15307, #22428, #20695 ) ) ;
#10388 = VERTEX_POINT ( 'NONE', #13698 ) ;
#10389 = CARTESIAN_POINT ( 'NONE',  ( 1.878215178124998497, -26.45312499938548711, 12.25316411605951927 ) ) ;
#10390 = CARTESIAN_POINT ( 'NONE',  ( 1.878215178125001605, 27.76562499938548711, 12.25316411605952283 ) ) ;
#10391 = CARTESIAN_POINT ( 'NONE',  ( 4.000000000000003553, 28.13124999877096855, 6.690598923241489970 ) ) ;
#10392 = AXIS2_PLACEMENT_3D ( 'NONE', #9913, #23919, #11998 ) ;
#10393 = CARTESIAN_POINT ( 'NONE',  ( -9.133673601486176352, 29.72853858738290711, 1.000000000000000000 ) ) ;
#10394 = EDGE_CURVE ( 'NONE', #4893, #19796, #8234, .T. ) ;
#10395 = AXIS2_PLACEMENT_3D ( 'NONE', #19009, #9067, #17050 ) ;
#10396 = CARTESIAN_POINT ( 'NONE',  ( 23.30358785661012888, 17.64673360711768169, 11.30940107675849760 ) ) ;
#10397 = CARTESIAN_POINT ( 'NONE',  ( 0.000000000000000000, -68.00000000000000000, 0.000000000000000000 ) ) ;
#10398 = CARTESIAN_POINT ( 'NONE',  ( 3.999999999999995559, -28.33750000000000213, 6.690598923241487306 ) ) ;
#10399 = DIRECTION ( 'NONE',  ( 0.000000000000000000, 0.000000000000000000, -1.000000000000000000 ) ) ;
#10400 = CARTESIAN_POINT ( 'NONE',  ( 26.00000000000000355, 3.184081677783117796E-15, 19.59999999999999787 ) ) ;
#10401 = AXIS2_PLACEMENT_3D ( 'NONE', #10844, #10590, #22242 ) ;
#10402 = CARTESIAN_POINT ( 'NONE',  ( -1.999999999999996669, 26.59374999877097423, 12.46410161513774639 ) ) ;
#10404 = ADVANCED_FACE ( 'NONE', ( #11737 ), #4283, .T. ) ;
#10403 = CARTESIAN_POINT ( 'NONE',  ( 17.93393197184562027, 20.59012934980492560, 12.25316411605951927 ) ) ;
#10405 = CARTESIAN_POINT ( 'NONE',  ( 19.30843454290614858, 19.30843454290607042, 4.381197846482986158 ) ) ;
#10406 = CARTESIAN_POINT ( 'NONE',  ( -3.999999999999995559, 28.33750000000000213, 6.690598923241487306 ) ) ;
#10407 = DIRECTION ( 'NONE',  ( 1.000000000000000000, 0.000000000000000000, 0.000000000000000000 ) ) ;
#10408 = CARTESIAN_POINT ( 'NONE',  ( 2.672651547586948120E-15, 25.47812499938548569, 13.33755215474602984 ) ) ;
#10409 = VECTOR ( 'NONE', #13550, 1000.000000000000000 ) ;
#10411 = VERTEX_POINT ( 'NONE', #23640 ) ;
#10410 = CARTESIAN_POINT ( 'NONE',  ( 0.000000000000000000, 0.000000000000000000, 1.000000000000000000 ) ) ;
#10412 = AXIS2_PLACEMENT_3D ( 'NONE', #23883, #15773, #19436 ) ;
#10413 = CYLINDRICAL_SURFACE ( 'NONE', #8306, 26.00000000000000711 ) ;
#10414 = CARTESIAN_POINT ( 'NONE',  ( 3.999999999999995559, -27.88750000000000284, 6.690598923241487306 ) ) ;
#10415 = ORIENTED_EDGE ( 'NONE', *, *, #23484, .T. ) ;
#10416 = DIRECTION ( 'NONE',  ( -0.000000000000000000, -0.000000000000000000, 1.000000000000000000 ) ) ;
#10417 = CARTESIAN_POINT ( 'NONE',  ( 4.000000000000001776, 26.25624999877096499, 11.30940107675849760 ) ) ;
#10418 = CARTESIAN_POINT ( 'NONE',  ( -1.878215178125000939, -26.86562499938548498, 12.25316411605952283 ) ) ;
#10420 = EDGE_LOOP ( 'NONE', ( #24466, #8775, #2248, #8573 ) ) ;
#10419 = DIRECTION ( 'NONE',  ( 0.000000000000000000, 0.000000000000000000, 1.000000000000000000 ) ) ;
#10421 = CIRCLE ( 'NONE', #11680, 31.10000000000000142 ) ;
#10422 = EDGE_CURVE ( 'NONE', #22500, #27, #16060, .T. ) ;
#10424 = ORIENTED_EDGE ( 'NONE', *, *, #7955, .T. ) ;
#10423 = AXIS2_PLACEMENT_3D ( 'NONE', #8157, #12596, #20573 ) ;
#10425 = CARTESIAN_POINT ( 'NONE',  ( -1.878215178125004048, -29.37812499938548783, 5.746835883940462963 ) ) ;
#10426 = EDGE_LOOP ( 'NONE', ( #19252, #20425, #25745, #6180 ) ) ;
#10427 = APPLICATION_CONTEXT ( 'automotive_design' ) ;
#10428 = ORIENTED_EDGE ( 'NONE', *, *, #14693, .T. ) ;
#10429 = EDGE_CURVE ( 'NONE', #15184, #22105, #12592, .T. ) ;
#10430 = CARTESIAN_POINT ( 'NONE',  ( 29.99470236596032535, 8.217531866531109230, -2.750000000000000000 ) ) ;
#10431 =( BOUNDED_CURVE ( )  B_SPLINE_CURVE ( 2, ( #11487, #25100, #17128, #15554, #13586, #7430, #7313, #15290, #25348 ),
 .UNSPECIFIED., .F., .F. ) 
 B_SPLINE_CURVE_WITH_KNOTS ( ( 3, 2, 2, 2, 3 ),
 ( 0.4750000000000000333, 0.4833333333333333370, 0.5000000000000000000, 0.5166666666666667185, 0.5250000000000000222 ),
 .UNSPECIFIED. ) 
 CURVE ( )  GEOMETRIC_REPRESENTATION_ITEM ( )  RATIONAL_B_SPLINE_CURVE ( ( 0.9330127018922194093, 0.9330127018922196314, 1.000000000000000000, 0.8660254037844387076, 1.000000000000000000, 0.8660254037844387076, 1.000000000000000000, 0.9330127018922194093, 0.9330127018922194093 ) ) 
 REPRESENTATION_ITEM ( '' )  );
#10432 = CARTESIAN_POINT ( 'NONE',  ( 3.756430356250002323, 25.66562499938548925, 11.16877607737301226 ) ) ;
#10433 = VECTOR ( 'NONE', #4969, 1000.000000000000000 ) ;
#10434 = CARTESIAN_POINT ( 'NONE',  ( -25.99307600111999150, 0.6000000000000000888, 20.00001200000000168 ) ) ;
#10435 = EDGE_CURVE ( 'NONE', #14766, #19279, #4642, .T. ) ;
#10436 =( BOUNDED_CURVE ( )  B_SPLINE_CURVE ( 2, ( #23849, #3974, #8159, #8032, #22144, #16016, #7765, #15747, #14047 ),
 .UNSPECIFIED., .F., .F. ) 
 B_SPLINE_CURVE_WITH_KNOTS ( ( 3, 2, 2, 2, 3 ),
 ( 0.1249999999999999861, 0.1333333333333333315, 0.1499999999999999944, 0.1666666666666666574, 0.1750000000000000167 ),
 .UNSPECIFIED. ) 
 CURVE ( )  GEOMETRIC_REPRESENTATION_ITEM ( )  RATIONAL_B_SPLINE_CURVE ( ( 0.9330127018922194093, 0.9330127018922192983, 1.000000000000000000, 0.8660254037844387076, 1.000000000000000000, 0.8660254037844387076, 1.000000000000000000, 0.9330127018922191873, 0.9330127018922194093 ) ) 
 REPRESENTATION_ITEM ( '' )  );
#10437 = VECTOR ( 'NONE', #11778, 1000.000000000000000 ) ;
#10438 = ADVANCED_FACE ( 'NONE', ( #4917 ), #4403, .T. ) ;
#10439 = CIRCLE ( 'NONE', #7529, 0.5000000000000004441 ) ;
#10440 = CARTESIAN_POINT ( 'NONE',  ( 3.756430356250002323, -11.16877607737301226, 2.915624999385482141 ) ) ;
#10441 = CARTESIAN_POINT ( 'NONE',  ( -1.878215178124995832, 25.29062499938548569, 5.746835883940462963 ) ) ;
#10442 = AXIS2_PLACEMENT_3D ( 'NONE', #11926, #16391, #17955 ) ;
#10443 = CARTESIAN_POINT ( 'NONE',  ( 0.000000000000000000, 0.000000000000000000, 0.000000000000000000 ) ) ;
#10444 = CARTESIAN_POINT ( 'NONE',  ( 3.469446951953614189E-15, 25.00000000000000000, 4.999999999999992006 ) ) ;
#10445 = CARTESIAN_POINT ( 'NONE',  ( 3.756430356250002323, 26.00312499938548427, 11.16877607737301403 ) ) ;
#10446 = FACE_OUTER_BOUND ( 'NONE', #11043, .T. ) ;
#10447 = CYLINDRICAL_SURFACE ( 'NONE', #21633, 0.5000000000000004441 ) ;
#10448 = CARTESIAN_POINT ( 'NONE',  ( 18.23451611984813425, 18.23451611984805609, 12.99999999999999112 ) ) ;
#10449 = CARTESIAN_POINT ( 'NONE',  ( -4.000000000000001776, -28.05624999877096926, 11.30940107675849760 ) ) ;
#10450 = CARTESIAN_POINT ( 'NONE',  ( 1.580380365229604700E-14, 27.58750000000000213, 12.99999999999999289 ) ) ;
#10451 = DIRECTION ( 'NONE',  ( 0.000000000000000000, 0.000000000000000000, 1.000000000000000000 ) ) ;
#10452 = CIRCLE ( 'NONE', #453, 31.10000000000000142 ) ;
#10453 = DIRECTION ( 'NONE',  ( 0.3681245526846875782, 0.9297764858882475725, 0.000000000000000000 ) ) ;
#10454 = CARTESIAN_POINT ( 'NONE',  ( 18.07541709408115693, 18.07541709408108233, 4.999999999999992006 ) ) ;
#10455 = ORIENTED_EDGE ( 'NONE', *, *, #546, .F. ) ;
#10456 = DIRECTION ( 'NONE',  ( 1.000000000000000000, 0.000000000000000000, 0.000000000000000000 ) ) ;
#10458 = ORIENTED_EDGE ( 'NONE', *, *, #18411, .T. ) ;
#10457 = CARTESIAN_POINT ( 'NONE',  ( 1.500000000000001776, -7.499999999999993783, 4.999999999999993783 ) ) ;
#10459 = AXIS2_PLACEMENT_3D ( 'NONE', #22381, #24217, #22263 ) ;
#10460 = VERTEX_POINT ( 'NONE', #20621 ) ;
#10461 = ORIENTED_EDGE ( 'NONE', *, *, #1035, .F. ) ;
#10462 = ORIENTED_EDGE ( 'NONE', *, *, #16679, .T. ) ;
#10463 = ORIENTED_EDGE ( 'NONE', *, *, #9599, .T. ) ;
#10464 = ORIENTED_EDGE ( 'NONE', *, *, #25796, .T. ) ;
#10465 = CARTESIAN_POINT ( 'NONE',  ( 0.7500000000000001110, 0.000000000000000000, 15.00000000000000178 ) ) ;
#10466 = AXIS2_PLACEMENT_3D ( 'NONE', #17259, #5467, #23516 ) ;
#10467 = ORIENTED_EDGE ( 'NONE', *, *, #10740, .F. ) ;
#10468 = EDGE_CURVE ( 'NONE', #24513, #380, #8469, .T. ) ;
#10469 = CARTESIAN_POINT ( 'NONE',  ( 26.49999999999999645, -0.5000000000000000000, 19.50000000000000000 ) ) ;
#10470 = CARTESIAN_POINT ( 'NONE',  ( 1.878215178125000939, 26.52812499938548285, 12.25316411605952283 ) ) ;
#10471 = ADVANCED_FACE ( 'NONE', ( #4801 ), #2966, .T. ) ;
#10472 = CARTESIAN_POINT ( 'NONE',  ( 1.878215178125000939, -12.25316411605952283, 1.978124999385485250 ) ) ;
#10473 = CARTESIAN_POINT ( 'NONE',  ( 30.45149776762729488, 6.317933499823327637, 1.000000000000000000 ) ) ;
#10474 = CARTESIAN_POINT ( 'NONE',  ( 21.67957950013421353, 16.36718474421539682, 11.16877607737301226 ) ) ;
#10475 = EDGE_CURVE ( 'NONE', #23470, #10990, #14605, .T. ) ;
#10476 = CIRCLE ( 'NONE', #12145, 0.5000000000000001110 ) ;
#10477 = CARTESIAN_POINT ( 'NONE',  ( 27.10000000000000142, 3.318792825689327485E-15, 1.000000000000000000 ) ) ;
#10478 = VECTOR ( 'NONE', #21674, 1000.000000000000000 ) ;
#10479 = CARTESIAN_POINT ( 'NONE',  ( 3.469446951953614189E-15, 35.50000000000000711, 8.999999999999992895 ) ) ;
#10480 = CARTESIAN_POINT ( 'NONE',  ( 1.878215178125000939, -12.25316411605952283, 1.865624999385483873 ) ) ;
#10481 = DIRECTION ( 'NONE',  ( 0.000000000000000000, 0.000000000000000000, 1.000000000000000000 ) ) ;
#10482 = CARTESIAN_POINT ( 'NONE',  ( -3.999999999999994671, 28.73124999877097352, 6.690598923241487306 ) ) ;
#10483 = CARTESIAN_POINT ( 'NONE',  ( 3.878215178125003604, 29.82343749907822783, 8.999999999999992895 ) ) ;
#10484 = VECTOR ( 'NONE', #15137, 1000.000000000000000 ) ;
#10485 = CARTESIAN_POINT ( 'NONE',  ( 3.735045420075836212E-15, -4.662447845253954171, 1.265624999385483118 ) ) ;
#10486 = CARTESIAN_POINT ( 'NONE',  ( -3.756430356250003655, -29.69687499938548569, 8.999999999999992895 ) ) ;
#10487 = DIRECTION ( 'NONE',  ( 1.000000000000000000, 0.000000000000000000, 0.000000000000000000 ) ) ;
#10488 = VERTEX_POINT ( 'NONE', #6886 ) ;
#10489 = ORIENTED_EDGE ( 'NONE', *, *, #9092, .F. ) ;
#10490 = CARTESIAN_POINT ( 'NONE',  ( 8.012344526598182026E-15, 28.51562499938549067, 4.662447845253954171 ) ) ;
#10491 = AXIS2_PLACEMENT_3D ( 'NONE', #12859, #25020, #20837 ) ;
#10492 = ORIENTED_EDGE ( 'NONE', *, *, #24097, .T. ) ;
#10493 = CYLINDRICAL_SURFACE ( 'NONE', #10840, 4.000000000000000000 ) ;
#10494 = VERTEX_POINT ( 'NONE', #22587 ) ;
#10495 = DIRECTION ( 'NONE',  ( 1.000000000000000000, 0.000000000000000000, 0.000000000000000000 ) ) ;
#10496 = ORIENTED_EDGE ( 'NONE', *, *, #8933, .F. ) ;
#10497 = CARTESIAN_POINT ( 'NONE',  ( -4.000000000000000000, 27.86874999877096926, 8.999999999999992895 ) ) ;
#10498 = AXIS2_PLACEMENT_3D ( 'NONE', #12751, #18371, #2409 ) ;
#10499 = VECTOR ( 'NONE', #4601, 1000.000000000000000 ) ;
#10500 = CARTESIAN_POINT ( 'NONE',  ( -3.999999999999995559, 29.18124999877096926, 6.690598923241487306 ) ) ;
#10501 = VERTEX_POINT ( 'NONE', #22322 ) ;
#10502 = CARTESIAN_POINT ( 'NONE',  ( 1.071796769724498999, 28.45134618820330275, 12.99999999999998757 ) ) ;
#10503 = CARTESIAN_POINT ( 'NONE',  ( 3.756430356250002323, 27.35312499938547859, 11.16877607737301226 ) ) ;
#10504 = CYLINDRICAL_SURFACE ( 'NONE', #15978, 0.5000000000000004441 ) ;
#10505 = AXIS2_PLACEMENT_3D ( 'NONE', #19785, #13645, #25676 ) ;
#10506 = EDGE_CURVE ( 'NONE', #23030, #14350, #18020, .T. ) ;
#10507 = CARTESIAN_POINT ( 'NONE',  ( 0.5000000000000000000, -2.999999999999999556, 20.00000000000000000 ) ) ;
#10508 = DIRECTION ( 'NONE',  ( -1.000000000000000000, 0.000000000000000000, 0.000000000000000000 ) ) ;
#10509 = CARTESIAN_POINT ( 'NONE',  ( 0.000000000000000000, 0.000000000000000000, 1.000000000000000000 ) ) ;
#10510 = CARTESIAN_POINT ( 'NONE',  ( 2.672651547586948120E-15, 28.17812499938548143, 13.33755215474602984 ) ) ;
#10511 = VECTOR ( 'NONE', #17535, 1000.000000000000000 ) ;
#10512 = AXIS2_PLACEMENT_3D ( 'NONE', #17678, #3800, #11780 ) ;
#10513 = EDGE_CURVE ( 'NONE', #25114, #256, #6243, .T. ) ;
#10514 = CARTESIAN_POINT ( 'NONE',  ( -3.999999999999996447, 26.12500000000000355, 8.999999999999992895 ) ) ;
#10515 = CARTESIAN_POINT ( 'NONE',  ( 2.620986760973688460E-15, -13.61880215351699874, 2.137499999999999734 ) ) ;
#10516 = AXIS2_PLACEMENT_3D ( 'NONE', #17846, #9604, #15887 ) ;
#10517 = CARTESIAN_POINT ( 'NONE',  ( -3.999999999999996447, 25.65624999877097423, 11.30940107675849404 ) ) ;
#10518 = CARTESIAN_POINT ( 'NONE',  ( -3.999999999999996447, 29.21874999877096712, 8.999999999999992895 ) ) ;
#10519 = AXIS2_PLACEMENT_3D ( 'NONE', #20882, #4531, #8595 ) ;
#10520 = CARTESIAN_POINT ( 'NONE',  ( 1.878215178124998497, -26.79062499938548214, 12.25316411605951927 ) ) ;
#10521 = CARTESIAN_POINT ( 'NONE',  ( -4.000000000000010658, -6.690598923241495299, 1.537500000000000311 ) ) ;
#10522 = ORIENTED_EDGE ( 'NONE', *, *, #19096, .F. ) ;
#10523 = CARTESIAN_POINT ( 'NONE',  ( 4.000000000000001776, 29.85624999877096997, 11.30940107675849760 ) ) ;
#10524 = CARTESIAN_POINT ( 'NONE',  ( 1.999999999999998224, -28.90000000000000213, 12.46410161513774639 ) ) ;
#10526 = VERTEX_POINT ( 'NONE', #4526 ) ;
#10525 = CARTESIAN_POINT ( 'NONE',  ( 1.878215178125005158, 27.12812499938548783, 5.746835883940462963 ) ) ;
#10527 = ORIENTED_EDGE ( 'NONE', *, *, #5334, .F. ) ;
#10528 = CARTESIAN_POINT ( 'NONE',  ( -16.23990935651735867, -26.52310962334733446, -2.750000000000000000 ) ) ;
#10529 = VECTOR ( 'NONE', #8772, 1000.000000000000000 ) ;
#10530 = CARTESIAN_POINT ( 'NONE',  ( -27.00874656207282953, 15.41874213889444079, -6.500000000000000000 ) ) ;
#10531 = ORIENTED_EDGE ( 'NONE', *, *, #7588, .T. ) ;
#10532 = ORIENTED_EDGE ( 'NONE', *, *, #14006, .T. ) ;
#10533 = CARTESIAN_POINT ( 'NONE',  ( -3.756430356250002323, -27.91562499938548569, 11.16877607737301403 ) ) ;
#10534 = CARTESIAN_POINT ( 'NONE',  ( -1.878215178124998275, 28.14062499938548711, 12.25316411605951927 ) ) ;
#10535 = DIRECTION ( 'NONE',  ( 0.000000000000000000, 0.000000000000000000, 1.000000000000000000 ) ) ;
#10536 = VECTOR ( 'NONE', #22491, 1000.000000000000000 ) ;
#10537 = CYLINDRICAL_SURFACE ( 'NONE', #18131, 0.5000000000000000000 ) ;
#10538 = EDGE_CURVE ( 'NONE', #18550, #1524, #10071, .T. ) ;
#10539 = CARTESIAN_POINT ( 'NONE',  ( 3.999999999999972466, -6.690598923241471319, 3.187499999999999556 ) ) ;
#10540 = SURFACE_STYLE_FILL_AREA ( #24926 ) ;
#10541 = CARTESIAN_POINT ( 'NONE',  ( 19.34820930021694352, 19.34820930021687246, 4.999999999999992006 ) ) ;
#10542 = CARTESIAN_POINT ( 'NONE',  ( 3.959305671612554781E-15, 30.00000000000000355, 12.99999999999999289 ) ) ;
#10543 = COLOUR_RGB ( '',0.8941176470588234615, 0.8941176470588234615, 0.8941176470588234615 ) ;
#10544 = DIRECTION ( 'NONE',  ( 0.000000000000000000, 0.000000000000000000, 1.000000000000000000 ) ) ;
#10545 = CARTESIAN_POINT ( 'NONE',  ( 20.74922837557196331, 18.09303099761251588, 5.746835883940462963 ) ) ;
#10546 = CARTESIAN_POINT ( 'NONE',  ( 20.90826363534070254, 18.07983651059444696, 12.46410161513774817 ) ) ;
#10547 = CARTESIAN_POINT ( 'NONE',  ( 3.834746474454188013E-15, 27.81249999999999645, 4.999999999999992006 ) ) ;
#10548 = DIRECTION ( 'NONE',  ( 0.000000000000000000, 1.000000000000000000, 0.000000000000000000 ) ) ;
#10549 = CARTESIAN_POINT ( 'NONE',  ( -3.756430356249997882, 29.11562499938548143, 11.16877607737301226 ) ) ;
#10550 = AXIS2_PLACEMENT_3D ( 'NONE', #13085, #23022, #5107 ) ;
#10552 = ORIENTED_EDGE ( 'NONE', *, *, #15269, .T. ) ;
#10551 = CARTESIAN_POINT ( 'NONE',  ( -0.2612076306139402004, 30.00000000000001066, 12.99999999999999467 ) ) ;
#10553 = CARTESIAN_POINT ( 'NONE',  ( -1.999999999999996669, 25.69374999877097920, 12.46410161513774639 ) ) ;
#10554 = CARTESIAN_POINT ( 'NONE',  ( 19.77367586078540995, 18.25792633293329104, 4.999999999999989342 ) ) ;
#10555 = EDGE_LOOP ( 'NONE', ( #6096, #12056, #15752, #4842, #13019, #23272, #8553, #12387, #20392, #16338, #7358, #21925, #6896, #15013, #20240, #12213, #16584, #1082, #11532, #2519, #7577, #24616, #16080, #4615 ) ) ;
#10556 = DIRECTION ( 'NONE',  ( 0.000000000000000000, 1.000000000000000000, 0.000000000000000000 ) ) ;
#10557 = CARTESIAN_POINT ( 'NONE',  ( -3.999999999999997335, 25.65624999877097068, 11.30940107675849404 ) ) ;
#10558 = CARTESIAN_POINT ( 'NONE',  ( -3.756430356250004099, -25.62812499938548072, 6.831223922626973533 ) ) ;
#10560 = VERTEX_POINT ( 'NONE', #10400 ) ;
#10559 = FACE_OUTER_BOUND ( 'NONE', #1278, .T. ) ;
#10561 = CARTESIAN_POINT ( 'NONE',  ( -3.469446951953614189E-15, -30.00000000000000355, 8.999999999999992895 ) ) ;
#10562 = AXIS2_PLACEMENT_3D ( 'NONE', #23160, #5743, #21703 ) ;
#10563 = VERTEX_POINT ( 'NONE', #2579 ) ;
#10564 = CARTESIAN_POINT ( 'NONE',  ( -3.735045420075836212E-15, -26.15312499938548285, 4.662447845253954171 ) ) ;
#10565 = ORIENTED_EDGE ( 'NONE', *, *, #9213, .T. ) ;
#10566 = ORIENTED_EDGE ( 'NONE', *, *, #19948, .F. ) ;
#10567 = DIRECTION ( 'NONE',  ( 0.000000000000000000, 0.000000000000000000, 1.000000000000000000 ) ) ;
#10568 = CARTESIAN_POINT ( 'NONE',  ( -3.756430356249996549, 25.47812499938548925, 8.999999999999992895 ) ) ;
#10569 = CARTESIAN_POINT ( 'NONE',  ( 2.000000000000000888, -12.46410161513774817, 3.468749998770968901 ) ) ;
#10570 = ADVANCED_FACE ( 'NONE', ( #743 ), #12649, .T. ) ;
#10571 = CARTESIAN_POINT ( 'NONE',  ( 3.735045420075836212E-15, -4.662447845253954171, 1.265624999385483118 ) ) ;
#10572 = CARTESIAN_POINT ( 'NONE',  ( -30.54913349766215802, 5.827558883616378083, 1.000000000000000000 ) ) ;
#10573 = CARTESIAN_POINT ( 'NONE',  ( 1.878215178125004048, 25.66562499938548569, 5.746835883940462963 ) ) ;
#10574 = EDGE_CURVE ( 'NONE', #6983, #17557, #15419, .T. ) ;
#10575 = CARTESIAN_POINT ( 'NONE',  ( 19.05342146176823093, 20.56917098962020418, 12.99999999999999645 ) ) ;
#10576 = LINE ( 'NONE', #20780, #19664 ) ;
#10577 = MECHANICAL_DESIGN_GEOMETRIC_PRESENTATION_REPRESENTATION (  '', ( #18128 ), #13936 ) ;
#10578 = CARTESIAN_POINT ( 'NONE',  ( 1.878215178125004048, 25.21562499938548285, 5.746835883940462963 ) ) ;
#10579 = CARTESIAN_POINT ( 'NONE',  ( 3.878215178125005380, 25.32343749907823138, 8.999999999999992895 ) ) ;
#10580 = CARTESIAN_POINT ( 'NONE',  ( 28.91604871112457076, -11.44867358849361416, -6.500000000000000000 ) ) ;
#10581 = EDGE_CURVE ( 'NONE', #4812, #12308, #18100, .T. ) ;
#10582 = CARTESIAN_POINT ( 'NONE',  ( -1.878215178125000939, -26.52812499938548285, 12.25316411605952283 ) ) ;
#10583 = FACE_OUTER_BOUND ( 'NONE', #10016, .T. ) ;
#10584 = CARTESIAN_POINT ( 'NONE',  ( -31.03863125411927371, -1.952785157361310198, -6.500000000000000000 ) ) ;
#10585 =( GEOMETRIC_REPRESENTATION_CONTEXT ( 3 ) GLOBAL_UNCERTAINTY_ASSIGNED_CONTEXT ( ( #13074 ) ) GLOBAL_UNIT_ASSIGNED_CONTEXT ( ( #2224, #24314, #21702 ) ) REPRESENTATION_CONTEXT ( 'NONE', 'WORKASPACE' ) );
#10586 = CARTESIAN_POINT ( 'NONE',  ( 3.834746474454188013E-15, 25.95624999877096428, 4.999999999999992006 ) ) ;
#10587 = CARTESIAN_POINT ( 'NONE',  ( 3.999903055931597784, -29.73215053696358368, 8.737301635141733414 ) ) ;
#10588 = EDGE_LOOP ( 'NONE', ( #11044, #21090, #11372, #6057 ) ) ;
#10589 = EDGE_CURVE ( 'NONE', #13396, #6968, #22524, .T. ) ;
#10590 = DIRECTION ( 'NONE',  ( 0.000000000000000000, -1.000000000000000000, 0.000000000000000000 ) ) ;
#10592 = ORIENTED_EDGE ( 'NONE', *, *, #1508, .T. ) ;
#10591 = CARTESIAN_POINT ( 'NONE',  ( -1.999999999999995781, -5.535898384862237620, 3.693749998770968546 ) ) ;
#10593 =( BOUNDED_CURVE ( )  B_SPLINE_CURVE ( 2, ( #7875, #3090, #18918, #5302, #11057, #3205, #14987, #12894, #1879 ),
 .UNSPECIFIED., .F., .F. ) 
 B_SPLINE_CURVE_WITH_KNOTS ( ( 3, 2, 2, 2, 3 ),
 ( 0.07500000000000001110, 0.08333333333333332871, 0.1000000000000000056, 0.1166666666666666685, 0.1250000000000000000 ),
 .UNSPECIFIED. ) 
 CURVE ( )  GEOMETRIC_REPRESENTATION_ITEM ( )  RATIONAL_B_SPLINE_CURVE ( ( 0.9330127018922192983, 0.9330127018922194093, 1.000000000000000000, 0.8660254037844387076, 1.000000000000000000, 0.8660254037844387076, 1.000000000000000000, 0.9330127018922194093, 0.9330127018922194093 ) ) 
 REPRESENTATION_ITEM ( '' )  );
#10594 = VERTEX_POINT ( 'NONE', #8542 ) ;
#10595 = ORIENTED_EDGE ( 'NONE', *, *, #12297, .T. ) ;
#10596 = ORIENTED_EDGE ( 'NONE', *, *, #11954, .T. ) ;
#10597 = VERTEX_POINT ( 'NONE', #18341 ) ;
#10598 = ORIENTED_EDGE ( 'NONE', *, *, #18971, .F. ) ;
#10599 = LINE ( 'NONE', #22646, #7207 ) ;
#10600 =( BOUNDED_CURVE ( )  B_SPLINE_CURVE ( 2, ( #14379, #22338, #20361, #514, #24823, #5320, #16858, #891, #1138 ),
 .UNSPECIFIED., .F., .F. ) 
 B_SPLINE_CURVE_WITH_KNOTS ( ( 3, 2, 2, 2, 3 ),
 ( 0.02500000000000000139, 0.03333333333333333287, 0.05000000000000000278, 0.06666666666666666574, 0.07500000000000001110 ),
 .UNSPECIFIED. ) 
 CURVE ( )  GEOMETRIC_REPRESENTATION_ITEM ( )  RATIONAL_B_SPLINE_CURVE ( ( 0.9330127018922194093, 0.9330127018922194093, 1.000000000000000000, 0.8660254037844387076, 1.000000000000000000, 0.8660254037844387076, 1.000000000000000000, 0.9330127018922191873, 0.9330127018922192983 ) ) 
 REPRESENTATION_ITEM ( '' )  );
#10601 =( GEOMETRIC_REPRESENTATION_CONTEXT ( 3 ) GLOBAL_UNCERTAINTY_ASSIGNED_CONTEXT ( ( #17261 ) ) GLOBAL_UNIT_ASSIGNED_CONTEXT ( ( #12116, #4399, #13832 ) ) REPRESENTATION_CONTEXT ( 'NONE', 'WORKASPACE' ) );
#10602 = VERTEX_POINT ( 'NONE', #2386 ) ;
#10603 = DIRECTION ( 'NONE',  ( 0.9048270524660262382, 0.4257792915650585042, 0.000000000000000000 ) ) ;
#10604 = CARTESIAN_POINT ( 'NONE',  ( 1.878215178125000939, 28.32812499938548711, 12.25316411605952283 ) ) ;
#10605 = CARTESIAN_POINT ( 'NONE',  ( -3.756430356249995661, -6.831223922626973533, 3.140624999385484006 ) ) ;
#10606 = CARTESIAN_POINT ( 'NONE',  ( 3.469446951953614189E-15, 35.50000000000000711, 8.999999999999992895 ) ) ;
#10607 = CARTESIAN_POINT ( 'NONE',  ( 22.23415261606371374, 19.57795523810426630, 12.25316411605952283 ) ) ;
#10608 = DIRECTION ( 'NONE',  ( 0.000000000000000000, -0.000000000000000000, 1.000000000000000000 ) ) ;
#10609 = CARTESIAN_POINT ( 'NONE',  ( 24.67207871933483432, -8.377607117416795646, 20.00001200000000523 ) ) ;
#10610 = ITEM_DEFINED_TRANSFORMATION ( 'NONE', 'NONE', #23581,  #21036 ) ;
#10611 = CARTESIAN_POINT ( 'NONE',  ( 3.756430356250004099, -6.831223922626973533, 1.978124999385481697 ) ) ;
#10612 = PRESENTATION_STYLE_ASSIGNMENT (( #25822 ) ) ;
#10613 = LINE ( 'NONE', #4751, #10499 ) ;
#10614 = CARTESIAN_POINT ( 'NONE',  ( 3.999999999999996447, -25.61874999877096926, 8.999999999999992895 ) ) ;
#10615 = CARTESIAN_POINT ( 'NONE',  ( 1.878215178125000939, -12.25316411605952283, 1.078124999385483784 ) ) ;
#10616 = DIRECTION ( 'NONE',  ( 1.000000000000000000, 0.000000000000000000, 0.000000000000000000 ) ) ;
#10617 = ORIENTED_EDGE ( 'NONE', *, *, #22743, .T. ) ;
#10618 = EDGE_CURVE ( 'NONE', #4929, #3732, #11569, .T. ) ;
#10619 = VERTEX_POINT ( 'NONE', #23608 ) ;
#10620 = CARTESIAN_POINT ( 'NONE',  ( -3.756430356249996105, 27.69062499938548427, 6.831223922626973533 ) ) ;
#10621 = EDGE_CURVE ( 'NONE', #10854, #14526, #16260, .T. ) ;
#10622 = ORIENTED_EDGE ( 'NONE', *, *, #9458, .F. ) ;
#10623 = FACE_BOUND ( 'NONE', #19524, .T. ) ;
#10624 = EDGE_LOOP ( 'NONE', ( #5702, #24649 ) ) ;
#10625 = CYLINDRICAL_SURFACE ( 'NONE', #869, 0.5000000000000004441 ) ;
#10626 = ORIENTED_EDGE ( 'NONE', *, *, #9292, .T. ) ;
#10627 = PLANE ( 'NONE',  #508 ) ;
#10628 = CARTESIAN_POINT ( 'NONE',  ( -5.827558883615604479, 30.54913349766230724, -6.500000000000000000 ) ) ;
#10629 = ORIENTED_EDGE ( 'NONE', *, *, #25723, .T. ) ;
#10630 = CARTESIAN_POINT ( 'NONE',  ( -1.998723687422152831E-12, 39.00000000001113420, 14.49999999998978240 ) ) ;
#10631 = CARTESIAN_POINT ( 'NONE',  ( 2.620986760973688460E-15, 25.33750000000000568, 13.61880215351699874 ) ) ;
#10632 = CARTESIAN_POINT ( 'NONE',  ( -3.137519842735244810E-15, 27.30624999877096926, 4.999999999999991118 ) ) ;
#10633 = CARTESIAN_POINT ( 'NONE',  ( 1.859271017917182139E-15, 26.68750000000000000, 12.99999999999999289 ) ) ;
#10634 = CARTESIAN_POINT ( 'NONE',  ( 15.93641908099185933, 21.59327333048416619, 6.690598923241487306 ) ) ;
#10635 = DIRECTION ( 'NONE',  ( 1.000000000000000000, 0.000000000000000000, 0.000000000000000000 ) ) ;
#10636 = B_SPLINE_CURVE_WITH_KNOTS ( 'NONE', 3,
 ( #18932, #24935, #9103, #7014, #15001, #1649, #1521, #15768, #17235, #21405, #21646, #23353, #5313, #9757, #17736, #25707, #15262, #3485 ),
 .UNSPECIFIED., .F., .F.,
 ( 4, 2, 2, 2, 2, 2, 2, 2, 4 ),
 ( 0.01878087663358380885, 0.01956282976579720376, 0.02034478289801060213, 0.02112673603022399704, 0.02190868916243739195, 0.02269064229465078686, 0.02347259542686418177, 0.02425454855907758014, 0.02503650169129097505 ),
 .UNSPECIFIED. ) ;
#10637 = CARTESIAN_POINT ( 'NONE',  ( 1.878215178125004048, 28.36562499938548143, 5.746835883940462963 ) ) ;
#10638 = EDGE_CURVE ( 'NONE', #6033, #13093, #4996, .T. ) ;
#10639 = CARTESIAN_POINT ( 'NONE',  ( -0.4150711328764303820, 38.77044187147116361, 3.285374590644589254 ) ) ;
#10640 = CARTESIAN_POINT ( 'NONE',  ( 0.000000000000000000, 0.000000000000000000, 1.000000000000000000 ) ) ;
#10641 = FACE_OUTER_BOUND ( 'NONE', #895, .T. ) ;
#10643 = EDGE_CURVE ( 'NONE', #7884, #23630, #15515, .T. ) ;
#10642 = CARTESIAN_POINT ( 'NONE',  ( 3.756430356249997438, -27.65312499938548640, 11.16877607737301048 ) ) ;
#10644 = CARTESIAN_POINT ( 'NONE',  ( -4.000000000000010658, -11.30940107675848694, 0.2624999999999985678 ) ) ;
#10645 = ORIENTED_EDGE ( 'NONE', *, *, #18717, .F. ) ;
#10646 = CARTESIAN_POINT ( 'NONE',  ( -3.756430356249996994, 26.37812499938548783, 8.999999999999992895 ) ) ;
#10647 = CARTESIAN_POINT ( 'NONE',  ( 3.999999999999996447, -29.27500000000000213, 8.999999999999992895 ) ) ;
#10649 = ORIENTED_EDGE ( 'NONE', *, *, #18730, .T. ) ;
#10648 = CARTESIAN_POINT ( 'NONE',  ( -3.756430356249997882, -11.16877607737301226, 0.4031249993854806868 ) ) ;
#10650 = ORIENTED_EDGE ( 'NONE', *, *, #5566, .T. ) ;
#10651 = CARTESIAN_POINT ( 'NONE',  ( 4.000000000000003553, -8.999999999999992895, 4.443749998770965881 ) ) ;
#10652 = DIRECTION ( 'NONE',  ( 1.000000000000000000, 0.000000000000000000, 0.000000000000000000 ) ) ;
#10653 = EDGE_LOOP ( 'NONE', ( #16917, #9472, #20117, #20638 ) ) ;
#10654 = CARTESIAN_POINT ( 'NONE',  ( -3.735045420075836212E-15, -25.81562499938548783, 4.662447845253954171 ) ) ;
#10655 = CYLINDRICAL_SURFACE ( 'NONE', #522, 4.000000000000000000 ) ;
#10656 = CARTESIAN_POINT ( 'NONE',  ( -1.071796769724492338, -28.90134618820330203, 12.99999999999999467 ) ) ;
#10657 = EDGE_CURVE ( 'NONE', #18582, #6126, #7579, .T. ) ;
#10658 = DIRECTION ( 'NONE',  ( 1.000000000000000000, 0.000000000000000000, 0.000000000000000000 ) ) ;
#10659 = CARTESIAN_POINT ( 'NONE',  ( 1.878215178125001605, 26.41562499938548925, 12.25316411605952283 ) ) ;
#10660 =( BOUNDED_CURVE ( )  B_SPLINE_CURVE ( 2, ( #2256, #20020, #24211, #22376, #22116, #15995, #14027, #13900, #24349, #6162, #20280, #4459, #12041, #34, #12434, #18089, #424, #4070, #6431, #6299, #14417, #3955, #20401, #2124, #4204, #168, #18470, #12182, #14292, #9956, #10332, #11920, #2502, #20156, #10470, #559, #8261, #15854, #23826, #10210, #10088, #23962, #5912, #16239, #22257, #21872, #16118, #292, #19890, #8140, #18210, #1989, #24080, #17948, #4338, #12313, #14150, #8009, #21993, #2377, #18327, #8393, #6044, #16384, #10856, #13098, #8777, #18709, #3027, #19095, #16626, #4591, #2761, #1062, #12712, #5122, #23035, #12570, #22649, #20549, #2642, #21073, #10604, #4737, #6820, #22507, #18593, #14532, #10723, #20679, #3151, #941, #16901, #10997, #681, #18979, #8530, #8648, #18851, #14803, #24591, #11116, #9036, #6678, #799, #2886, #22778, #20944, #4855, #17020, #14669, #15060, #16766, #24735, #12830, #20805, #8921, #4984, #24985, #24865, #6947 ),
 .UNSPECIFIED., .F., .F. ) 
 B_SPLINE_CURVE_WITH_KNOTS ( ( 3, 2, 2, 2, 2, 2, 2, 2, 2, 2, 2, 2, 2, 2, 2, 2, 2, 2, 2, 2, 2, 2, 2, 2, 2, 2, 2, 2, 2, 2, 2, 2, 2, 2, 2, 2, 2, 2, 2, 2, 2, 2, 2, 2, 2, 2, 2, 2, 2, 2, 2, 2, 2, 2, 2, 2, 2, 2, 2, 2, 3 ),
 ( 0.000000000000000000, 0.01666666666666666644, 0.03333333333333333287, 0.05000000000000000278, 0.06666666666666666574, 0.08333333333333332871, 0.1000000000000000056, 0.1166666666666666685, 0.1333333333333333315, 0.1499999999999999944, 0.1666666666666666574, 0.1833333333333333204, 0.2000000000000000111, 0.2166666666666666741, 0.2333333333333333370, 0.2500000000000000000, 0.2666666666666666630, 0.2833333333333333259, 0.2999999999999999889, 0.3166666666666666519, 0.3333333333333333148, 0.3499999999999999778, 0.3666666666666666408, 0.3833333333333333592, 0.4000000000000000222, 0.4166666666666666852, 0.4333333333333333481, 0.4500000000000000111, 0.4666666666666666741, 0.4833333333333333370, 0.5000000000000000000, 0.5166666666666667185, 0.5333333333333333259, 0.5500000000000000444, 0.5666666666666666519, 0.5833333333333333703, 0.5999999999999999778, 0.6166666666666666963, 0.6333333333333333037, 0.6500000000000000222, 0.6666666666666666297, 0.6833333333333333481, 0.6999999999999999556, 0.7166666666666666741, 0.7333333333333332815, 0.7500000000000000000, 0.7666666666666667185, 0.7833333333333333259, 0.8000000000000000444, 0.8166666666666666519, 0.8333333333333333703, 0.8499999999999999778, 0.8666666666666666963, 0.8833333333333333037, 0.9000000000000000222, 0.9166666666666666297, 0.9333333333333333481, 0.9499999999999999556, 0.9666666666666666741, 0.9833333333333332815, 1.000000000000000000 ),
 .UNSPECIFIED. ) 
 CURVE ( )  GEOMETRIC_REPRESENTATION_ITEM ( )  RATIONAL_B_SPLINE_CURVE ( ( 1.000000000000000000, 0.8660254037844387076, 1.000000000000000000, 0.8660254037844387076, 1.000000000000000000, 0.8660254037844387076, 1.000000000000000000, 0.8660254037844387076, 1.000000000000000000, 0.8660254037844387076, 1.000000000000000000, 0.8660254037844387076, 1.000000000000000000, 0.8660254037844387076, 1.000000000000000000, 0.8660254037844387076, 1.000000000000000000, 0.8660254037844387076, 1.000000000000000000, 0.8660254037844387076, 1.000000000000000000, 0.8660254037844387076, 1.000000000000000000, 0.8660254037844387076, 1.000000000000000000, 0.8660254037844387076, 1.000000000000000000, 0.8660254037844387076, 1.000000000000000000, 0.8660254037844387076, 1.000000000000000000, 0.8660254037844387076, 1.000000000000000000, 0.8660254037844387076, 1.000000000000000000, 0.8660254037844387076, 1.000000000000000000, 0.8660254037844387076, 1.000000000000000000, 0.8660254037844387076, 1.000000000000000000, 0.8660254037844387076, 1.000000000000000000, 0.8660254037844387076, 1.000000000000000000, 0.8660254037844387076, 1.000000000000000000, 0.8660254037844387076, 1.000000000000000000, 0.8660254037844387076, 1.000000000000000000, 0.8660254037844387076, 1.000000000000000000, 0.8660254037844387076, 1.000000000000000000, 0.8660254037844387076, 1.000000000000000000, 0.8660254037844387076, 1.000000000000000000, 0.8660254037844387076, 1.000000000000000000, 0.8660254037844387076, 1.000000000000000000, 0.8660254037844387076, 1.000000000000000000, 0.8660254037844387076, 1.000000000000000000, 0.8660254037844387076, 1.000000000000000000, 0.8660254037844387076, 1.000000000000000000, 0.8660254037844387076, 1.000000000000000000, 0.8660254037844387076, 1.000000000000000000, 0.8660254037844387076, 1.000000000000000000, 0.8660254037844387076, 1.000000000000000000, 0.8660254037844387076, 1.000000000000000000, 0.8660254037844387076, 1.000000000000000000, 0.8660254037844387076, 1.000000000000000000, 0.8660254037844387076, 1.000000000000000000, 0.8660254037844387076, 1.000000000000000000, 0.8660254037844387076, 1.000000000000000000, 0.8660254037844387076, 1.000000000000000000, 0.8660254037844387076, 1.000000000000000000, 0.8660254037844387076, 1.000000000000000000, 0.8660254037844387076, 1.000000000000000000, 0.8660254037844387076, 1.000000000000000000, 0.8660254037844387076, 1.000000000000000000, 0.8660254037844387076, 1.000000000000000000, 0.8660254037844387076, 1.000000000000000000, 0.8660254037844387076, 1.000000000000000000, 0.8660254037844387076, 1.000000000000000000, 0.8660254037844387076, 1.000000000000000000, 0.8660254037844387076, 1.000000000000000000, 0.8660254037844387076, 1.000000000000000000, 0.8660254037844387076, 1.000000000000000000, 0.8660254037844387076, 1.000000000000000000 ) ) 
 REPRESENTATION_ITEM ( '' )  );
#10661 = CARTESIAN_POINT ( 'NONE',  ( 3.878215178125003604, 25.32343749907822783, 8.999999999999992895 ) ) ;
#10662 = CARTESIAN_POINT ( 'NONE',  ( 0.000000000000000000, -43.00000000000000000, 0.000000000000000000 ) ) ;
#10663 = CARTESIAN_POINT ( 'NONE',  ( 31.06601413805602263, 1.453535542772627087, 1.000000000000000000 ) ) ;
#10664 = CARTESIAN_POINT ( 'NONE',  ( 5.577813053751546416E-15, 25.95624999877097139, 4.999999999999992006 ) ) ;
#10665 = CARTESIAN_POINT ( 'NONE',  ( -1.878215178124998497, 25.44062499938548427, 12.25316411605951927 ) ) ;
#10666 = DIRECTION ( 'NONE',  ( 0.000000000000000000, 0.000000000000000000, 1.000000000000000000 ) ) ;
#10667 = CARTESIAN_POINT ( 'NONE',  ( 17.21571288163933389, 22.52810763755800849, 11.16877607737301226 ) ) ;
#10668 = CARTESIAN_POINT ( 'NONE',  ( 23.67481891673307715, 18.01796466724061574, 6.690598923241489970 ) ) ;
#10669 = DIRECTION ( 'NONE',  ( 0.000000000000000000, 0.000000000000000000, -1.000000000000000000 ) ) ;
#10670 = EDGE_CURVE ( 'NONE', #12491, #2759, #20959, .T. ) ;
#10671 = DIRECTION ( 'NONE',  ( -1.000000000000000000, 0.000000000000000000, 0.000000000000000000 ) ) ;
#10672 = CARTESIAN_POINT ( 'NONE',  ( 1.878215178125004048, 28.92812499938548854, 5.746835883940462963 ) ) ;
#10674 = VERTEX_POINT ( 'NONE', #16913 ) ;
#10673 = CARTESIAN_POINT ( 'NONE',  ( 5.577813053751546416E-15, 28.20624999877096784, 4.999999999999992006 ) ) ;
#10675 = CARTESIAN_POINT ( 'NONE',  ( 15.57168961538060969, 20.88408437129928785, 6.831223922626973533 ) ) ;
#10676 = CARTESIAN_POINT ( 'NONE',  ( -3.999999999999996447, -8.999999999999992895, 1.125000000000000888 ) ) ;
#10677 = VECTOR ( 'NONE', #18355, 1000.000000000000000 ) ;
#10678 = ORIENTED_EDGE ( 'NONE', *, *, #15223, .T. ) ;
#10679 = DIRECTION ( 'NONE',  ( 0.000000000000000000, 0.000000000000000000, 1.000000000000000000 ) ) ;
#10680 = CARTESIAN_POINT ( 'NONE',  ( -1.999999999999995781, 27.34374999877097068, 5.535898384862237620 ) ) ;
#10681 = CARTESIAN_POINT ( 'NONE',  ( -3.756430356250003655, -26.94062499938548427, 8.999999999999992895 ) ) ;
#10683 = ORIENTED_EDGE ( 'NONE', *, *, #18911, .T. ) ;
#10682 = CARTESIAN_POINT ( 'NONE',  ( -12.78762572734076919, -28.34936733434192035, -2.750000000000000000 ) ) ;
#10684 = CARTESIAN_POINT ( 'NONE',  ( 31.00322564728514507, 2.451530025009026392, -6.500000000000000000 ) ) ;
#10685 = EDGE_CURVE ( 'NONE', #19796, #12137, #24113, .T. ) ;
#10686 = ORIENTED_EDGE ( 'NONE', *, *, #7865, .T. ) ;
#10687 = CARTESIAN_POINT ( 'NONE',  ( -3.756430356250004099, -26.97812499938548569, 6.831223922626973533 ) ) ;
#10688 = ORIENTED_EDGE ( 'NONE', *, *, #24086, .F. ) ;
#10689 = PRODUCT_DEFINITION_SHAPE ( 'NONE', 'NONE',  #9821 ) ;
#10690 = ORIENTED_EDGE ( 'NONE', *, *, #14808, .T. ) ;
#10691 = CARTESIAN_POINT ( 'NONE',  ( -29.57785765677917311, 9.610428525061202265, -6.500000000000000000 ) ) ;
#10692 = CARTESIAN_POINT ( 'NONE',  ( -3.756430356249997882, 25.92812499938548854, 8.999999999999992895 ) ) ;
#10693 = EDGE_CURVE ( 'NONE', #16373, #16896, #474, .T. ) ;
#10694 = CARTESIAN_POINT ( 'NONE',  ( 2.000000000000000888, 27.62500000000000000, 12.46410161513774817 ) ) ;
#10695 = CARTESIAN_POINT ( 'NONE',  ( 3.756430356250004099, -6.831223922626973533, 2.090624999385480631 ) ) ;
#10696 = CARTESIAN_POINT ( 'NONE',  ( -3.110308778861381462, 38.49999999999999289, 3.869115154270378554 ) ) ;
#10697 = CARTESIAN_POINT ( 'NONE',  ( 3.756430356250003655, 27.39062499938548356, 8.999999999999992895 ) ) ;
#10698 = DIRECTION ( 'NONE',  ( -0.000000000000000000, -0.000000000000000000, 1.000000000000000000 ) ) ;
#10699 = CARTESIAN_POINT ( 'NONE',  ( 1.057460391440397258E-14, -28.71250000000000213, 4.999999999999992006 ) ) ;
#10700 = UNCERTAINTY_MEASURE_WITH_UNIT (LENGTH_MEASURE( 1.000000000000000082E-05 ), #1847, 'distance_accuracy_value', 'NONE');
#10701 = CARTESIAN_POINT ( 'NONE',  ( 1.878215178125000939, 28.66562499938548569, 12.25316411605952283 ) ) ;
#10702 = LINE ( 'NONE', #6657, #24652 ) ;
#10703 = CARTESIAN_POINT ( 'NONE',  ( 1.071796769724494558, 25.93615380933863435, 4.999999999999992895 ) ) ;
#10704 = CARTESIAN_POINT ( 'NONE',  ( -1.071796769724487230, 28.67634618820330417, 4.999999999999992006 ) ) ;
#10705 = CARTESIAN_POINT ( 'NONE',  ( -1.878215178125000939, -27.42812499938548498, 12.25316411605952283 ) ) ;
#10706 = CARTESIAN_POINT ( 'NONE',  ( 1.878215178125004048, 29.37812499938548783, 5.746835883940462963 ) ) ;
#10707 = DIRECTION ( 'NONE',  ( 0.000000000000000000, 1.000000000000000000, 0.000000000000000000 ) ) ;
#10708 = CARTESIAN_POINT ( 'NONE',  ( -5.577813053751546416E-15, -25.33750000000000213, 12.99999999999999289 ) ) ;
#10709 = CARTESIAN_POINT ( 'NONE',  ( -1.999999999999998224, 28.00000000000000000, 12.46410161513774639 ) ) ;
#10710 = EDGE_LOOP ( 'NONE', ( #9354, #338, #15749, #22804, #19348, #19905 ) ) ;
#10711 = CARTESIAN_POINT ( 'NONE',  ( 3.469446951953614189E-15, 30.00000000000000355, 8.999999999999992895 ) ) ;
#10713 = EDGE_LOOP ( 'NONE', ( #20297, #645, #24228, #15115 ) ) ;
#10712 = LINE ( 'NONE', #8519, #24593 ) ;
#10715 = ORIENTED_EDGE ( 'NONE', *, *, #7734, .F. ) ;
#10714 = EDGE_CURVE ( 'NONE', #20266, #89, #8657, .T. ) ;
#10716 = ORIENTED_EDGE ( 'NONE', *, *, #17537, .F. ) ;
#10717 = VERTEX_POINT ( 'NONE', #24997 ) ;
#10718 = VERTEX_POINT ( 'NONE', #7085 ) ;
#10719 = CARTESIAN_POINT ( 'NONE',  ( 3.469446951953614189E-15, 30.00000000000000355, 8.999999999999992895 ) ) ;
#10720 = ADVANCED_FACE ( 'NONE', ( #6833 ), #20564, .F. ) ;
#10721 = ORIENTED_EDGE ( 'NONE', *, *, #10670, .T. ) ;
#10722 = CARTESIAN_POINT ( 'NONE',  ( 0.000000000000000000, 0.000000000000000000, 17.69999999999999929 ) ) ;
#10723 = CARTESIAN_POINT ( 'NONE',  ( -1.878215178124995832, 28.55312499938548498, 5.746835883940462963 ) ) ;
#10724 = CARTESIAN_POINT ( 'NONE',  ( -1.878215178124995832, -5.746835883940462963, 3.553124999385485427 ) ) ;
#10725 = DIRECTION ( 'NONE',  ( 0.000000000000000000, 0.000000000000000000, 1.000000000000000000 ) ) ;
#10726 = CARTESIAN_POINT ( 'NONE',  ( 19.10065816080342671, 21.75685553876272493, 5.746835883940462963 ) ) ;
#10727 = EDGE_CURVE ( 'NONE', #21926, #21953, #15073, .T. ) ;
#10728 = DIRECTION ( 'NONE',  ( 0.000000000000000000, 0.000000000000000000, 1.000000000000000000 ) ) ;
#10729 = CARTESIAN_POINT ( 'NONE',  ( 25.83240171513484285, -3.403349963601437267, 20.00001200000000168 ) ) ;
#10730 = CARTESIAN_POINT ( 'NONE',  ( 1.878215178125000939, -12.25316411605952283, 3.215624999385484184 ) ) ;
#10731 = DIRECTION ( 'NONE',  ( 1.000000000000000000, 0.000000000000000000, 0.000000000000000000 ) ) ;
#10732 = CARTESIAN_POINT ( 'NONE',  ( -1.071796769724481901, 27.96115380933863293, 12.99999999999999645 ) ) ;
#10733 = CARTESIAN_POINT ( 'NONE',  ( 2.620986760973688460E-15, 29.38749999999999929, 13.61880215351699874 ) ) ;
#10734 =( BOUNDED_CURVE ( )  B_SPLINE_CURVE ( 2, ( #10276, #1934, #11736, #4141, #21811, #24142, #23639, #356, #11981 ),
 .UNSPECIFIED., .F., .F. ) 
 B_SPLINE_CURVE_WITH_KNOTS ( ( 3, 2, 2, 2, 3 ),
 ( 0.8250000000000000666, 0.8333333333333333703, 0.8499999999999999778, 0.8666666666666666963, 0.8750000000000000000 ),
 .UNSPECIFIED. ) 
 CURVE ( )  GEOMETRIC_REPRESENTATION_ITEM ( )  RATIONAL_B_SPLINE_CURVE ( ( 0.9330127018922194093, 0.9330127018922198534, 1.000000000000000000, 0.8660254037844387076, 1.000000000000000000, 0.8660254037844387076, 1.000000000000000000, 0.9330127018922194093, 0.9330127018922194093 ) ) 
 REPRESENTATION_ITEM ( '' )  );
#10735 = CARTESIAN_POINT ( 'NONE',  ( -1.071796769724491671, 29.57634618820330275, 4.999999999999995559 ) ) ;
#10736 = CARTESIAN_POINT ( 'NONE',  ( -3.756430356249996994, -8.999999999999992895, 0.9281249993854829849 ) ) ;
#10737 = CARTESIAN_POINT ( 'NONE',  ( -1.071796769724494558, -28.24240381056766580, 4.999999999999992895 ) ) ;
#10738 = DIRECTION ( 'NONE',  ( 0.000000000000000000, 0.000000000000000000, 1.000000000000000000 ) ) ;
#10739 = EDGE_LOOP ( 'NONE', ( #23116, #7610, #18974, #19113 ) ) ;
#10740 = EDGE_CURVE ( 'NONE', #19876, #20539, #22789, .T. ) ;
#10741 = ORIENTED_EDGE ( 'NONE', *, *, #532, .F. ) ;
#10742 = CARTESIAN_POINT ( 'NONE',  ( -3.756430356249994773, 29.07812499938548711, 8.999999999999992895 ) ) ;
#10743 =( BOUNDED_CURVE ( )  B_SPLINE_CURVE ( 2, ( #12786, #11327, #3352, #13048, #15264, #8869, #13294, #1405, #23232 ),
 .UNSPECIFIED., .F., .F. ) 
 B_SPLINE_CURVE_WITH_KNOTS ( ( 3, 2, 2, 2, 3 ),
 ( 0.5750000000000000666, 0.5833333333333333703, 0.5999999999999999778, 0.6166666666666666963, 0.6250000000000000000 ),
 .UNSPECIFIED. ) 
 CURVE ( )  GEOMETRIC_REPRESENTATION_ITEM ( )  RATIONAL_B_SPLINE_CURVE ( ( 0.9330127018922194093, 0.9330127018922198534, 1.000000000000000000, 0.8660254037844387076, 1.000000000000000000, 0.8660254037844387076, 1.000000000000000000, 0.9330127018922194093, 0.9330127018922194093 ) ) 
 REPRESENTATION_ITEM ( '' )  );
#10744 = ORIENTED_EDGE ( 'NONE', *, *, #3069, .T. ) ;
#10745 = DIRECTION ( 'NONE',  ( 0.000000000000000000, 0.000000000000000000, 1.000000000000000000 ) ) ;
#10746 = ORIENTED_EDGE ( 'NONE', *, *, #18146, .F. ) ;
#10747 = CARTESIAN_POINT ( 'NONE',  ( 3.756430356249997882, -25.96562499938548640, 11.16877607737301226 ) ) ;
#10748 = VERTEX_POINT ( 'NONE', #4865 ) ;
#10749 = CARTESIAN_POINT ( 'NONE',  ( 1.533898589781675205E-14, 27.98124999877097352, 12.99999999999999289 ) ) ;
#10750 = EDGE_LOOP ( 'NONE', ( #12562, #16232, #3677, #24467 ) ) ;
#10751 = DIRECTION ( 'NONE',  ( 0.000000000000000000, 0.000000000000000000, 1.000000000000000000 ) ) ;
#10752 = EDGE_CURVE ( 'NONE', #125, #21679, #10867, .T. ) ;
#10753 = CARTESIAN_POINT ( 'NONE',  ( -1.878215178124995832, 29.34062499938548285, 5.746835883940462963 ) ) ;
#10754 = DIRECTION ( 'NONE',  ( 0.000000000000000000, 1.000000000000000000, 0.000000000000000000 ) ) ;
#10755 = AXIS2_PLACEMENT_3D ( 'NONE', #4082, #5927, #11931 ) ;
#10756 = DIRECTION ( 'NONE',  ( -0.000000000000000000, -1.000000000000000000, -0.000000000000000000 ) ) ;
#10757 = CARTESIAN_POINT ( 'NONE',  ( 1.500000000000000222, 0.000000000000000000, 17.69999999999999929 ) ) ;
#10758 = CARTESIAN_POINT ( 'NONE',  ( 16.92403133439988139, 22.23642609031855244, 6.831223922626973533 ) ) ;
#10759 = EDGE_CURVE ( 'NONE', #16184, #17145, #8935, .T. ) ;
#10760 = EDGE_CURVE ( 'NONE', #4269, #5905, #2900, .T. ) ;
#10761 = CARTESIAN_POINT ( 'NONE',  ( 2.672651547586948120E-15, 29.07812499938548001, 13.33755215474602984 ) ) ;
#10762 = CARTESIAN_POINT ( 'NONE',  ( 16.74068927859332234, 19.39688665655263122, 12.25316411605951927 ) ) ;
#10763 = LINE ( 'NONE', #6722, #16619 ) ;
#10764 = ORIENTED_EDGE ( 'NONE', *, *, #23066, .F. ) ;
#10765 = CARTESIAN_POINT ( 'NONE',  ( -4.000000000000026645, -6.690598923241505958, 3.281249998770966680 ) ) ;
#10766 = CARTESIAN_POINT ( 'NONE',  ( -1.999999999999996669, 26.14374999877097494, 12.46410161513774639 ) ) ;
#10767 = DIRECTION ( 'NONE',  ( 0.000000000000000000, 0.000000000000000000, 1.000000000000000000 ) ) ;
#10768 = CARTESIAN_POINT ( 'NONE',  ( -3.756430356250003655, -26.94062499938548427, 8.999999999999992895 ) ) ;
#10769 = CARTESIAN_POINT ( 'NONE',  ( 4.000000000000003553, -8.999999999999992895, 0.4499999999999990119 ) ) ;
#10770 = CARTESIAN_POINT ( 'NONE',  ( -3.756430356249995661, 25.89062499938548356, 6.831223922626973533 ) ) ;
#10771 = CYLINDRICAL_SURFACE ( 'NONE', #5436, 4.000000000000000000 ) ;
#10773 = ORIENTED_EDGE ( 'NONE', *, *, #17833, .T. ) ;
#10772 = CARTESIAN_POINT ( 'NONE',  ( 0.000000000000000000, 29.64062499938549422, 13.33755215474603162 ) ) ;
#10774 = VERTEX_POINT ( 'NONE', #955 ) ;
#10775 = CARTESIAN_POINT ( 'NONE',  ( 4.648177544792954952E-15, 25.73124999877097707, 12.99999999999999289 ) ) ;
#10776 = AXIS2_PLACEMENT_3D ( 'NONE', #691, #10481, #4863 ) ;
#10777 = EDGE_LOOP ( 'NONE', ( #2783, #11141, #12205, #22891 ) ) ;
#10778 = CARTESIAN_POINT ( 'NONE',  ( -1.878215178125000939, -26.07812499938548356, 12.25316411605952283 ) ) ;
#10779 = CARTESIAN_POINT ( 'NONE',  ( 1.878215178125003382, 29.56562499938549138, 12.25316411605952283 ) ) ;
#10780 = CARTESIAN_POINT ( 'NONE',  ( 1.878215178125006934, 25.21562499938548996, 5.746835883940462963 ) ) ;
#10781 = FACE_OUTER_BOUND ( 'NONE', #20038, .T. ) ;
#10782 = CARTESIAN_POINT ( 'NONE',  ( -1.999999999999993117, 25.60000000000000497, 5.535898384862237620 ) ) ;
#10783 = ADVANCED_FACE ( 'NONE', ( #21084 ), #1755, .F. ) ;
#10784 = EDGE_CURVE ( 'NONE', #16676, #18610, #19340, .T. ) ;
#10785 = CARTESIAN_POINT ( 'NONE',  ( -1.878215178124998497, -12.25316411605951927, 4.490624999385482319 ) ) ;
#10786 = VECTOR ( 'NONE', #18549, 1000.000000000000000 ) ;
#10787 = CARTESIAN_POINT ( 'NONE',  ( 3.526711513754847704, 29.50000000000000000, 13.85410196624967405 ) ) ;
#10788 = VECTOR ( 'NONE', #24147, 1000.000000000000000 ) ;
#10789 = DIRECTION ( 'NONE',  ( 0.000000000000000000, 0.000000000000000000, 1.000000000000000000 ) ) ;
#10790 = CARTESIAN_POINT ( 'NONE',  ( 3.999999999999996447, -28.37500000000000000, 8.999999999999992895 ) ) ;
#10791 = EDGE_CURVE ( 'NONE', #24696, #16618, #13407, .T. ) ;
#10792 = AXIS2_PLACEMENT_3D ( 'NONE', #9220, #3079, #15118 ) ;
#10793 = DIRECTION ( 'NONE',  ( -0.000000000000000000, -0.000000000000000000, 1.000000000000000000 ) ) ;
#10794 = CARTESIAN_POINT ( 'NONE',  ( -3.756430356249996105, 25.32812499938548356, 6.831223922626973533 ) ) ;
#10795 = AXIS2_PLACEMENT_3D ( 'NONE', #1727, #15324, #13367 ) ;
#10796 = CARTESIAN_POINT ( 'NONE',  ( -29.72853858738291422, -9.133673601486165694, -2.750000000000000000 ) ) ;
#10797 = CARTESIAN_POINT ( 'NONE',  ( 21.73261250872320716, 16.42021775280438689, 6.831223922626973533 ) ) ;
#10798 = CARTESIAN_POINT ( 'NONE',  ( 23.93998395967802750, 18.28312971018556965, 11.30940107675849760 ) ) ;
#10799 = CARTESIAN_POINT ( 'NONE',  ( 2.000000000000003997, 27.77500000000000213, 5.535898384862238508 ) ) ;
#10800 = CARTESIAN_POINT ( 'NONE',  ( -5.532151103383211144, 38.49999999999999289, 11.32277940608570255 ) ) ;
#10801 = CARTESIAN_POINT ( 'NONE',  ( 3.756430356250002323, 26.90312499938548640, 11.16877607737301226 ) ) ;
#10802 = FACE_OUTER_BOUND ( 'NONE', #16504, .T. ) ;
#10803 = CARTESIAN_POINT ( 'NONE',  ( 19.79463422097012426, 17.13843684301067682, 5.746835883940462963 ) ) ;
#10804 = CARTESIAN_POINT ( 'NONE',  ( 3.469446951953614189E-15, 30.00000000000000355, 8.999999999999992895 ) ) ;
#10805 = VERTEX_POINT ( 'NONE', #23391 ) ;
#10806 = DIRECTION ( 'NONE',  ( -1.000000000000000000, 0.000000000000000000, 0.000000000000000000 ) ) ;
#10807 = CARTESIAN_POINT ( 'NONE',  ( -3.999999999999996003, 26.93124999877096926, 6.690598923241487306 ) ) ;
#10808 = CARTESIAN_POINT ( 'NONE',  ( -3.756430356250002323, -27.80312499938548143, 11.16877607737301226 ) ) ;
#10810 = ORIENTED_EDGE ( 'NONE', *, *, #10839, .T. ) ;
#10809 = CYLINDRICAL_SURFACE ( 'NONE', #21705, 0.5000000000000004441 ) ;
#10811 = CARTESIAN_POINT ( 'NONE',  ( 3.959305671612554781E-15, 30.00000000000000355, 12.99999999999999289 ) ) ;
#10812 = CIRCLE ( 'NONE', #12920, 31.10000000000000142 ) ;
#10813 = ORIENTED_EDGE ( 'NONE', *, *, #21784, .T. ) ;
#10814 = CARTESIAN_POINT ( 'NONE',  ( -1.878215178125004048, -26.11562499938548498, 5.746835883940462963 ) ) ;
#10815 = ORIENTED_EDGE ( 'NONE', *, *, #2794, .F. ) ;
#10816 = ORIENTED_EDGE ( 'NONE', *, *, #15631, .T. ) ;
#10817 = DIRECTION ( 'NONE',  ( 1.000000000000000000, 0.000000000000000000, 0.000000000000000000 ) ) ;
#10818 = CARTESIAN_POINT ( 'NONE',  ( -3.756430356249996549, 26.82812499938549067, 8.999999999999992895 ) ) ;
#10819 = AXIS2_PLACEMENT_3D ( 'NONE', #23945, #20386, #22635 ) ;
#10820 = CARTESIAN_POINT ( 'NONE',  ( -3.999999999999996447, -8.999999999999992895, 2.024999999999999023 ) ) ;
#10821 = EDGE_CURVE ( 'NONE', #12737, #10488, #3517, .T. ) ;
#10822 = EDGE_CURVE ( 'NONE', #6671, #21954, #19461, .T. ) ;
#10823 = CIRCLE ( 'NONE', #8329, 6.000000000000000000 ) ;
#10824 = CARTESIAN_POINT ( 'NONE',  ( -1.878215178124998497, -12.25316411605951927, 2.803124999385484539 ) ) ;
#10825 = FILL_AREA_STYLE ('',( #22618 ) ) ;
#10826 = AXIS2_PLACEMENT_3D ( 'NONE', #1513, #15513, #17084 ) ;
#10827 = CARTESIAN_POINT ( 'NONE',  ( 3.756430356250003655, 27.84062499938548640, 8.999999999999992895 ) ) ;
#10828 = CARTESIAN_POINT ( 'NONE',  ( 22.00869856443133088, 19.18027143968506465, 5.535898384862238508 ) ) ;
#10829 = AXIS2_PLACEMENT_3D ( 'NONE', #20499, #254, #8222 ) ;
#10830 = DIRECTION ( 'NONE',  ( -0.8763066800438602533, 0.4817536741017213187, 0.000000000000000000 ) ) ;
#10831 = CARTESIAN_POINT ( 'NONE',  ( 3.735045420075836212E-15, 27.95312499938548001, 4.662447845253954171 ) ) ;
#10832 = CARTESIAN_POINT ( 'NONE',  ( 3.469446951953614189E-15, 30.00000000000000355, 8.999999999999992895 ) ) ;
#10833 = DIRECTION ( 'NONE',  ( 0.000000000000000000, 1.000000000000000000, 0.000000000000000000 ) ) ;
#10834 = CARTESIAN_POINT ( 'NONE',  ( 17.67766952966372429, 17.67766952966365679, 8.999999999999992895 ) ) ;
#10835 = CARTESIAN_POINT ( 'NONE',  ( -2.672651547586948120E-15, -27.84062499938548640, 13.33755215474602984 ) ) ;
#10836 = CARTESIAN_POINT ( 'NONE',  ( 0.000000000000000000, 0.000000000000000000, 1.000000000000000000 ) ) ;
#10837 = VECTOR ( 'NONE', #11862, 1000.000000000000000 ) ;
#10839 = EDGE_CURVE ( 'NONE', #19344, #4678, #10476, .T. ) ;
#10838 = DIRECTION ( 'NONE',  ( 1.000000000000000000, 0.000000000000000000, 0.000000000000000000 ) ) ;
#10841 = CARTESIAN_POINT ( 'NONE',  ( 3.469446951953614189E-15, -8.999999999999992895, 18.00000000000000000 ) ) ;
#10840 = AXIS2_PLACEMENT_3D ( 'NONE', #8549, #18351, #4227 ) ;
#10842 = CARTESIAN_POINT ( 'NONE',  ( -2.000000000000003997, -28.67500000000000426, 5.535898384862238508 ) ) ;
#10843 = VERTEX_POINT ( 'NONE', #13587 ) ;
#10844 = CARTESIAN_POINT ( 'NONE',  ( -3.469446951953614189E-15, -25.00000000000000000, 8.999999999999992895 ) ) ;
#10846 = ORIENTED_EDGE ( 'NONE', *, *, #4360, .F. ) ;
#10845 = DIRECTION ( 'NONE',  ( -0.4817536741017063306, 0.8763066800438685799, 0.000000000000000000 ) ) ;
#10847 = ORIENTED_EDGE ( 'NONE', *, *, #11148, .F. ) ;
#10848 = VECTOR ( 'NONE', #14791, 1000.000000000000000 ) ;
#10849 = EDGE_LOOP ( 'NONE', ( #13213, #20083, #23061, #15725 ) ) ;
#10850 = ORIENTED_EDGE ( 'NONE', *, *, #10953, .T. ) ;
#10851 = ORIENTED_EDGE ( 'NONE', *, *, #9696, .T. ) ;
#10852 = DIRECTION ( 'NONE',  ( 0.000000000000000000, 0.000000000000000000, 1.000000000000000000 ) ) ;
#10853 =( BOUNDED_CURVE ( )  B_SPLINE_CURVE ( 2, ( #8846, #20741, #18777, #4517, #8704, #18265, #22317, #866, #16834 ),
 .UNSPECIFIED., .F., .F. ) 
 B_SPLINE_CURVE_WITH_KNOTS ( ( 3, 2, 2, 2, 3 ),
 ( 0.2750000000000000222, 0.2833333333333333259, 0.2999999999999999889, 0.3166666666666666519, 0.3250000000000000111 ),
 .UNSPECIFIED. ) 
 CURVE ( )  GEOMETRIC_REPRESENTATION_ITEM ( )  RATIONAL_B_SPLINE_CURVE ( ( 0.9330127018922194093, 0.9330127018922196314, 1.000000000000000000, 0.8660254037844387076, 1.000000000000000000, 0.8660254037844387076, 1.000000000000000000, 0.9330127018922191873, 0.9330127018922194093 ) ) 
 REPRESENTATION_ITEM ( '' )  );
#10854 = VERTEX_POINT ( 'NONE', #3635 ) ;
#10855 = CARTESIAN_POINT ( 'NONE',  ( 4.000000000000003553, 25.19687499938548925, 8.999999999999992895 ) ) ;
#10856 = CARTESIAN_POINT ( 'NONE',  ( -1.878215178124995832, 27.65312499938548640, 5.746835883940462963 ) ) ;
#10857 = VECTOR ( 'NONE', #5367, 1000.000000000000000 ) ;
#10858 = CARTESIAN_POINT ( 'NONE',  ( 3.735045420075836212E-15, -4.662447845253954171, 4.415624999385481253 ) ) ;
#10859 = DIRECTION ( 'NONE',  ( -0.000000000000000000, 1.000000000000000000, -0.000000000000000000 ) ) ;
#10860 = CARTESIAN_POINT ( 'NONE',  ( 22.56362157461194329, -13.02991752792603819, 20.00001200000000523 ) ) ;
#10861 = VECTOR ( 'NONE', #9289, 1000.000000000000000 ) ;
#10863 = EDGE_CURVE ( 'NONE', #22864, #5788, #11539, .T. ) ;
#10862 = CARTESIAN_POINT ( 'NONE',  ( -1.999999999999998224, -12.46410161513774639, 0.3000000000000016542 ) ) ;
#10864 = DIRECTION ( 'NONE',  ( -0.9921147013144785420, -0.1253332335642980688, 0.000000000000000000 ) ) ;
#10865 = CARTESIAN_POINT ( 'NONE',  ( -30.24338421796775123, 7.248980000274508839, -6.500000000000000000 ) ) ;
#10866 = DIRECTION ( 'NONE',  ( 0.000000000000000000, 1.000000000000000000, 0.000000000000000000 ) ) ;
#10867 = LINE ( 'NONE', #18867, #18018 ) ;
#10868 = CARTESIAN_POINT ( 'NONE',  ( 1.878215178125004048, -5.746835883940462963, 2.578124999385485339 ) ) ;
#10869 = FACE_OUTER_BOUND ( 'NONE', #3580, .T. ) ;
#10870 = FACE_OUTER_BOUND ( 'NONE', #7763, .T. ) ;
#10871 = VERTEX_POINT ( 'NONE', #5991 ) ;
#10872 = CLOSED_SHELL ( 'NONE', ( #7503, #19417, #19156, #8197, #18807, #384, #22572, #14915, #22018, #7032, #18992, #11887, #22585, #16071, #9332, #4836, #22699, #3771, #9541, #13204, #20309, #4025, #1486, #8510, #12361, #7223, #13896, #20583, #25286, #24751, #2606, #20998, #1435, #12760, #21847, #3854, #21362, #1605, #5839, #6286, #8903, #5375, #16448, #22360, #14147, #17505, #61, #12625, #8771, #7788, #7164, #20648, #8564, #18534, #25716, #1093, #11559 ) ) ;
#10873 = ORIENTED_EDGE ( 'NONE', *, *, #14943, .F. ) ;
#10874 = CIRCLE ( 'NONE', #7116, 6.000000000000000000 ) ;
#10875 = ORIENTED_EDGE ( 'NONE', *, *, #5541, .F. ) ;
#10876 = DIRECTION ( 'NONE',  ( 1.000000000000000000, -0.000000000000000000, -0.000000000000000000 ) ) ;
#10877 = ORIENTED_EDGE ( 'NONE', *, *, #13602, .T. ) ;
#10878 = CARTESIAN_POINT ( 'NONE',  ( -3.756430356250004099, -26.64062499938549067, 6.831223922626973533 ) ) ;
#10879 = VERTEX_POINT ( 'NONE', #23769 ) ;
#10880 = CARTESIAN_POINT ( 'NONE',  ( 3.469446951953614189E-15, 30.00000000000000355, 8.999999999999992895 ) ) ;
#10881 = AXIS2_PLACEMENT_3D ( 'NONE', #9770, #17746, #23890 ) ;
#10882 = ORIENTED_EDGE ( 'NONE', *, *, #15492, .T. ) ;
#10883 = CARTESIAN_POINT ( 'NONE',  ( 3.469446951953614189E-15, 39.50000000000000000, 8.999999999999992895 ) ) ;
#10884 = CARTESIAN_POINT ( 'NONE',  ( -1.878215178124995832, 28.44062499938548427, 5.746835883940462963 ) ) ;
#10885 = CARTESIAN_POINT ( 'NONE',  ( 23.96296185032708337, 19.82388608118420237, -6.500000000000000000 ) ) ;
#10886 = CIRCLE ( 'NONE', #20934, 31.10000000000000142 ) ;
#10887 = CIRCLE ( 'NONE', #24258, 26.00000000000000711 ) ;
#10888 = CARTESIAN_POINT ( 'NONE',  ( 2.000000000000000888, 26.27499999999999858, 12.46410161513774817 ) ) ;
#10889 = CARTESIAN_POINT ( 'NONE',  ( -1.071796769724481901, 28.41115380933862866, 12.99999999999999645 ) ) ;
#10890 = CARTESIAN_POINT ( 'NONE',  ( 19.68629472953723436, 19.68629472953716686, 13.33755215474602984 ) ) ;
#10891 = VECTOR ( 'NONE', #4014, 1000.000000000000000 ) ;
#10892 = CARTESIAN_POINT ( 'NONE',  ( -30.85476721088022600, 3.897863563850190616, -6.500000000000000000 ) ) ;
#10893 = CARTESIAN_POINT ( 'NONE',  ( 1.878215178125000939, 27.76562499938548356, 12.25316411605952283 ) ) ;
#10894 =( BOUNDED_CURVE ( )  B_SPLINE_CURVE ( 2, ( #11009, #5134, #3159, #9434, #9172 ),
 .UNSPECIFIED., .F., .F. ) 
 B_SPLINE_CURVE_WITH_KNOTS ( ( 3, 2, 3 ),
 ( 0.9749999999999999778, 0.9833333333333332815, 1.000000000000000000 ),
 .UNSPECIFIED. ) 
 CURVE ( )  GEOMETRIC_REPRESENTATION_ITEM ( )  RATIONAL_B_SPLINE_CURVE ( ( 0.9330127018922194093, 0.9330127018922194093, 1.000000000000000000, 0.8660254037844387076, 1.000000000000000000 ) ) 
 REPRESENTATION_ITEM ( '' )  );
#10895 = EDGE_CURVE ( 'NONE', #7827, #15156, #21821, .T. ) ;
#10896 = CARTESIAN_POINT ( 'NONE',  ( 20.40451381974352074, 17.74831644178408041, 12.25316411605952283 ) ) ;
#10897 = CARTESIAN_POINT ( 'NONE',  ( -21.65113613650359525, -22.32573188046897172, -6.500000000000000000 ) ) ;
#10898 = AXIS2_PLACEMENT_3D ( 'NONE', #20439, #2537, #18506 ) ;
#10899 = ORIENTED_EDGE ( 'NONE', *, *, #23472, .F. ) ;
#10900 = EDGE_CURVE ( 'NONE', #4850, #12001, #19327, .T. ) ;
#10901 = DIRECTION ( 'NONE',  ( 0.000000000000000000, 0.000000000000000000, 1.000000000000000000 ) ) ;
#10902 = B_SPLINE_CURVE_WITH_KNOTS ( 'NONE', 3,
 ( #21041, #19443, #16985, #7029, #1030, #3231, #24949, #9006, #15017, #13451, #7546, #7300, #3501, #7416, #1146, #3117, #17109, #9118, #9391, #5327, #22997, #10959, #21420, #11473, #15279, #5082, #11082, #1537, #19063, #25084, #7171, #11202, #15160, #5211 ),
 .UNSPECIFIED., .F., .F.,
 ( 4, 2, 2, 2, 2, 2, 2, 2, 2, 2, 2, 2, 2, 2, 2, 2, 4 ),
 ( 0.000000000000000000, 0.0007824850735655044642, 0.001564970147131008928, 0.002347455220696513176, 0.003129940294262017857, 0.003912425367827522538, 0.004694910441393026351, 0.005477395514958531032, 0.006259880588524035713, 0.007042365662089540394, 0.007824850735655045075, 0.008607335809220548889, 0.009389820882786052703, 0.01017230595635155825, 0.01095479102991706206, 0.01173727610348256761, 0.01251976117704807143 ),
 .UNSPECIFIED. ) ;
#10903 = AXIS2_PLACEMENT_3D ( 'NONE', #5071, #4813, #16585 ) ;
#10904 = CARTESIAN_POINT ( 'NONE',  ( -1.878215178125000939, -27.31562499938548427, 12.25316411605952283 ) ) ;
#10905 = AXIS2_PLACEMENT_3D ( 'NONE', #17260, #25228, #11481 ) ;
#10906 = CARTESIAN_POINT ( 'NONE',  ( 0.000000000000000000, 0.000000000000000000, -6.500000000000000000 ) ) ;
#10907 = CARTESIAN_POINT ( 'NONE',  ( 2.000000000000000888, 28.91874999877096997, 12.46410161513774817 ) ) ;
#10908 = CARTESIAN_POINT ( 'NONE',  ( 0.2902671272941750868, 30.00000000000000355, 12.99999999999999112 ) ) ;
#10909 = ADVANCED_FACE ( 'NONE', ( #4409 ), #4022, .F. ) ;
#10911 = ORIENTED_EDGE ( 'NONE', *, *, #15065, .T. ) ;
#10910 = CARTESIAN_POINT ( 'NONE',  ( 1.878215178125003382, 29.37812499938548783, 5.746835883940462963 ) ) ;
#10912 = ORIENTED_EDGE ( 'NONE', *, *, #20906, .F. ) ;
#10913 = DIRECTION ( 'NONE',  ( 0.000000000000000000, 0.000000000000000000, -1.000000000000000000 ) ) ;
#10914 = AXIS2_PLACEMENT_3D ( 'NONE', #13166, #22971, #15373 ) ;
#10915 = DIRECTION ( 'NONE',  ( 0.000000000000000000, 0.000000000000000000, 1.000000000000000000 ) ) ;
#10916 = ORIENTED_EDGE ( 'NONE', *, *, #6754, .T. ) ;
#10917 = B_SPLINE_CURVE_WITH_KNOTS ( 'NONE', 3,
 ( #18306, #12811, #20783, #18827, #2356, #8509, #916, #777, #16742, #24710 ),
 .UNSPECIFIED., .F., .F.,
 ( 4, 2, 2, 2, 4 ),
 ( 0.01251976117704807143, 0.01338929815772731124, 0.01425883513840654933, 0.01512837211908578741, 0.01599790909976502723 ),
 .UNSPECIFIED. ) ;
#10918 = CARTESIAN_POINT ( 'NONE',  ( 3.756430356249996994, -29.07812499938548356, 8.999999999999992895 ) ) ;
#10919 = DIRECTION ( 'NONE',  ( -0.000000000000000000, -1.000000000000000000, 0.000000000000000000 ) ) ;
#10920 = CARTESIAN_POINT ( 'NONE',  ( 0.000000000000000000, 25.92812499938548854, 13.33755215474603162 ) ) ;
#10921 = EDGE_CURVE ( 'NONE', #22990, #21955, #10886, .T. ) ;
#10922 = CIRCLE ( 'NONE', #22624, 0.4999999999999997780 ) ;
#10923 = CARTESIAN_POINT ( 'NONE',  ( -1.071796769724494558, -26.38615380933864074, 4.999999999999992895 ) ) ;
#10924 = CARTESIAN_POINT ( 'NONE',  ( -1.878215178124998275, 28.59062499938548640, 12.25316411605951927 ) ) ;
#10925 = CIRCLE ( 'NONE', #15966, 0.5000000000000009992 ) ;
#10926 = CIRCLE ( 'NONE', #23064, 31.10000000000000142 ) ;
#10927 =( REPRESENTATION_RELATIONSHIP ('NONE','NONE', #25031, #13517 ) REPRESENTATION_RELATIONSHIP_WITH_TRANSFORMATION ( #20288 )SHAPE_REPRESENTATION_RELATIONSHIP( ) );
#10928 = FACE_OUTER_BOUND ( 'NONE', #5646, .T. ) ;
#10929 = DIRECTION ( 'NONE',  ( 0.000000000000000000, -1.000000000000000000, 0.000000000000000000 ) ) ;
#10930 = DIRECTION ( 'NONE',  ( 0.9685831611286337406, 0.2486898871648445808, 0.000000000000000000 ) ) ;
#10931 = VECTOR ( 'NONE', #22270, 1000.000000000000000 ) ;
#10932 = LINE ( 'NONE', #8711, #22195 ) ;
#10933 = CARTESIAN_POINT ( 'NONE',  ( 3.735045420075836212E-15, 25.25312499938548427, 4.662447845253954171 ) ) ;
#10934 = DIRECTION ( 'NONE',  ( -0.000000000000000000, -0.000000000000000000, 1.000000000000000000 ) ) ;
#10935 = CARTESIAN_POINT ( 'NONE',  ( 20.50609665440990526, 14.84924240491746339, 8.999999999999992895 ) ) ;
#10936 = CARTESIAN_POINT ( 'NONE',  ( 21.81216202160668871, 16.49976726568787200, 6.831223922626973533 ) ) ;
#10937 = CARTESIAN_POINT ( 'NONE',  ( 1.071796769724494558, 27.79240381056766651, 4.999999999999992895 ) ) ;
#10938 = DIRECTION ( 'NONE',  ( 1.000000000000000000, 0.000000000000000000, 0.000000000000000000 ) ) ;
#10939 = CARTESIAN_POINT ( 'NONE',  ( 3.735045420075836212E-15, 28.85312499938548569, 4.662447845253954171 ) ) ;
#10940 = DIRECTION ( 'NONE',  ( 0.000000000000000000, 0.000000000000000000, 1.000000000000000000 ) ) ;
#10941 = AXIS2_PLACEMENT_3D ( 'NONE', #2084, #23662, #8108 ) ;
#10942 = CARTESIAN_POINT ( 'NONE',  ( 22.31597560320210505, 17.00358084728328478, 11.16877607737301403 ) ) ;
#10943 = CARTESIAN_POINT ( 'NONE',  ( 21.65113613650343538, 22.32573188046912449, -2.750000000000000000 ) ) ;
#10944 = ORIENTED_EDGE ( 'NONE', *, *, #4324, .F. ) ;
#10945 = DIRECTION ( 'NONE',  ( 1.000000000000000000, 0.000000000000000000, 0.000000000000000000 ) ) ;
#10946 = CARTESIAN_POINT ( 'NONE',  ( 4.000000000000001776, 27.15624999877097423, 11.30940107675849760 ) ) ;
#10947 = CARTESIAN_POINT ( 'NONE',  ( 3.756430356249996994, -28.51562499938548356, 8.999999999999992895 ) ) ;
#10948 = ADVANCED_FACE ( 'NONE', ( #14097 ), #4149, .F. ) ;
#10950 = ORIENTED_EDGE ( 'NONE', *, *, #2339, .T. ) ;
#10949 = CARTESIAN_POINT ( 'NONE',  ( 5.577813053751546416E-15, 25.73124999877097352, 12.99999999999999289 ) ) ;
#10951 = VECTOR ( 'NONE', #11864, 1000.000000000000000 ) ;
#10952 = CARTESIAN_POINT ( 'NONE',  ( 18.67203843983824996, 18.67203843983818246, 4.999999999999991118 ) ) ;
#10953 = EDGE_CURVE ( 'NONE', #20598, #2083, #18163, .T. ) ;
#10954 = CIRCLE ( 'NONE', #1780, 0.5000000000000006661 ) ;
#10955 = ORIENTED_EDGE ( 'NONE', *, *, #10759, .T. ) ;
#10956 = CARTESIAN_POINT ( 'NONE',  ( 1.878215178124995832, -27.09062499938548640, 5.746835883940462963 ) ) ;
#10957 = ORIENTED_EDGE ( 'NONE', *, *, #19375, .F. ) ;
#10958 = ORIENTED_EDGE ( 'NONE', *, *, #13384, .F. ) ;
#10959 = CARTESIAN_POINT ( 'NONE',  ( 18.51809052069471306, 23.60276563550342388, 10.77252090037689136 ) ) ;
#10960 = ADVANCED_FACE ( 'NONE', ( #242 ), #366, .T. ) ;
#10961 = CARTESIAN_POINT ( 'NONE',  ( -3.756430356249997882, 28.62812499938548783, 8.999999999999992895 ) ) ;
#10962 = DIRECTION ( 'NONE',  ( -0.000000000000000000, -0.000000000000000000, 1.000000000000000000 ) ) ;
#10963 = AXIS2_PLACEMENT_3D ( 'NONE', #23893, #5709, #2185 ) ;
#10964 = CARTESIAN_POINT ( 'NONE',  ( -3.756430356249995661, -6.831223922626973533, 1.340624999385481075 ) ) ;
#10965 = CARTESIAN_POINT ( 'NONE',  ( 23.26836714124207361, 18.93629030671969460, 11.57226653943512851 ) ) ;
#10966 = CARTESIAN_POINT ( 'NONE',  ( -3.756430356249995661, 28.02812499938548640, 6.831223922626973533 ) ) ;
#10967 = CIRCLE ( 'NONE', #22673, 0.4999999999999999445 ) ;
#10968 = CARTESIAN_POINT ( 'NONE',  ( -29.09636799667067564, 10.98232076577254368, -2.750000000000000000 ) ) ;
#10969 = CARTESIAN_POINT ( 'NONE',  ( 1.071796769724493448, -28.73259618943232852, 4.999999999999995559 ) ) ;
#10970 = UNCERTAINTY_MEASURE_WITH_UNIT (LENGTH_MEASURE( 1.000000000000000082E-05 ), #23012, 'distance_accuracy_value', 'NONE');
#10971 = UNCERTAINTY_MEASURE_WITH_UNIT (LENGTH_MEASURE( 1.000000000000000082E-05 ), #231, 'distance_accuracy_value', 'NONE');
#10972 = CYLINDRICAL_SURFACE ( 'NONE', #4967, 4.000000000000000000 ) ;
#10973 = PRESENTATION_STYLE_ASSIGNMENT (( #20918 ) ) ;
#10974 = FACE_OUTER_BOUND ( 'NONE', #3584, .T. ) ;
#10975 = DIRECTION ( 'NONE',  ( -6.938893903907225222E-15, -1.000000000000000000, 0.000000000000000000 ) ) ;
#10976 = CYLINDRICAL_SURFACE ( 'NONE', #17212, 4.000000000000000000 ) ;
#10977 = CARTESIAN_POINT ( 'NONE',  ( -1.878215178125000939, -27.87812499938548427, 12.25316411605952283 ) ) ;
#10978 = DIRECTION ( 'NONE',  ( 1.000000000000000000, 0.000000000000000000, 0.000000000000000000 ) ) ;
#10979 = CARTESIAN_POINT ( 'NONE',  ( -1.999999999999995781, 29.59374999877096712, 5.535898384862237620 ) ) ;
#10980 = AXIS2_PLACEMENT_3D ( 'NONE', #12077, #12344, #2156 ) ;
#10981 = CARTESIAN_POINT ( 'NONE',  ( -24.00000000000000355, 2.939152317953648289E-15, 19.00000000000000000 ) ) ;
#10982 = ADVANCED_FACE ( 'NONE', ( #16186 ), #6242, .F. ) ;
#10983 = CARTESIAN_POINT ( 'NONE',  ( 2.440392720584789288, -29.90136469312441037, 12.17998752022640296 ) ) ;
#10984 = ORIENTED_EDGE ( 'NONE', *, *, #14381, .F. ) ;
#10985 = CARTESIAN_POINT ( 'NONE',  ( 20.47307855473466631, 15.16068379881585138, 8.999999999999992895 ) ) ;
#10987 = ORIENTED_EDGE ( 'NONE', *, *, #23354, .F. ) ;
#10986 = DIRECTION ( 'NONE',  ( 1.000000000000000000, 0.000000000000000000, 0.000000000000000000 ) ) ;
#10988 = EDGE_CURVE ( 'NONE', #22563, #446, #17941, .T. ) ;
#10989 = AXIS2_PLACEMENT_3D ( 'NONE', #11628, #23067, #25015 ) ;
#10990 = VERTEX_POINT ( 'NONE', #4532 ) ;
#10991 = ORIENTED_EDGE ( 'NONE', *, *, #714, .T. ) ;
#10992 = ORIENTED_EDGE ( 'NONE', *, *, #10422, .F. ) ;
#10993 = ORIENTED_EDGE ( 'NONE', *, *, #13854, .F. ) ;
#10994 = CARTESIAN_POINT ( 'NONE',  ( -1.626862140677534194E-14, -27.58750000000000213, 12.99999999999999289 ) ) ;
#10995 = EDGE_LOOP ( 'NONE', ( #11076, #11556, #14886, #16161 ) ) ;
#10996 = DIRECTION ( 'NONE',  ( 1.000000000000000000, 0.000000000000000000, 0.000000000000000000 ) ) ;
#10997 = CARTESIAN_POINT ( 'NONE',  ( 2.672651547586948120E-15, 28.74062499938548854, 13.33755215474603162 ) ) ;
#10998 = EDGE_CURVE ( 'NONE', #13848, #16720, #14251, .T. ) ;
#10999 = PRESENTATION_LAYER_ASSIGNMENT (  '', '', ( #2661 ) ) ;
#11000 = CARTESIAN_POINT ( 'NONE',  ( 3.735045420075836212E-15, -4.662447845253954171, 1.153124999385480187 ) ) ;
#11001 = DIRECTION ( 'NONE',  ( 0.000000000000000000, 0.000000000000000000, 1.000000000000000000 ) ) ;
#11002 = CARTESIAN_POINT ( 'NONE',  ( 8.000000000000000000, 10.00000000000000000, 17.00000000000000000 ) ) ;
#11003 = CARTESIAN_POINT ( 'NONE',  ( 1.878215178125000939, 25.62812499938548783, 12.25316411605952283 ) ) ;
#11004 = AXIS2_PLACEMENT_3D ( 'NONE', #10883, #16926, #24894 ) ;
#11005 = CARTESIAN_POINT ( 'NONE',  ( -1.999999999999995781, -5.535898384862237620, 0.5999999999999998668 ) ) ;
#11006 = CARTESIAN_POINT ( 'NONE',  ( -3.756430356249995661, -6.831223922626973533, 3.478124999385480809 ) ) ;
#11007 = CARTESIAN_POINT ( 'NONE',  ( -3.878215178125003604, -25.07031249969274356, 8.999999999999992895 ) ) ;
#11008 = DIRECTION ( 'NONE',  ( -0.000000000000000000, -0.000000000000000000, -1.000000000000000000 ) ) ;
#11009 = CARTESIAN_POINT ( 'NONE',  ( -1.859271017917182139E-15, -29.38749999999999929, 12.99999999999999289 ) ) ;
#11010 = CARTESIAN_POINT ( 'NONE',  ( -3.999999999999994671, 29.70624999877097139, 11.30940107675849404 ) ) ;
#11011 = CARTESIAN_POINT ( 'NONE',  ( -3.756430356249996105, -6.831223922626973533, 3.590624999385483740 ) ) ;
#11012 = LINE ( 'NONE', #21086, #16222 ) ;
#11013 = CARTESIAN_POINT ( 'NONE',  ( -1.999999999999995781, 25.60000000000000142, 5.535898384862237620 ) ) ;
#11014 = ORIENTED_EDGE ( 'NONE', *, *, #18566, .F. ) ;
#11015 = ORIENTED_EDGE ( 'NONE', *, *, #16755, .T. ) ;
#11016 = ORIENTED_EDGE ( 'NONE', *, *, #21604, .T. ) ;
#11017 = DIRECTION ( 'NONE',  ( -1.000000000000000000, 0.000000000000000000, -0.000000000000000000 ) ) ;
#11018 = ORIENTED_EDGE ( 'NONE', *, *, #11945, .F. ) ;
#11019 = CYLINDRICAL_SURFACE ( 'NONE', #20474, 0.5000000000000004441 ) ;
#11020 = ORIENTED_EDGE ( 'NONE', *, *, #8349, .F. ) ;
#11021 = DIRECTION ( 'NONE',  ( 0.000000000000000000, 0.000000000000000000, 1.000000000000000000 ) ) ;
#11022 = ADVANCED_FACE ( 'NONE', ( #747 ), #6891, .T. ) ;
#11023 = CIRCLE ( 'NONE', #18964, 6.000000000000000000 ) ;
#11024 = ORIENTED_EDGE ( 'NONE', *, *, #13478, .T. ) ;
#11025 = CARTESIAN_POINT ( 'NONE',  ( 26.25859848311271705, 16.66421332384673804, 1.000000000000000000 ) ) ;
#11026 = CARTESIAN_POINT ( 'NONE',  ( 3.756430356250002323, 29.15312499938548640, 11.16877607737301226 ) ) ;
#11027 = DIRECTION ( 'NONE',  ( -0.000000000000000000, -0.000000000000000000, 1.000000000000000000 ) ) ;
#11028 = CARTESIAN_POINT ( 'NONE',  ( -29.09636799667091367, -10.98232076577190774, -6.500000000000000000 ) ) ;
#11029 = CARTESIAN_POINT ( 'NONE',  ( -20.78941499438242246, -22.67092431280570963, 1.000000000000000000 ) ) ;
#11030 = CARTESIAN_POINT ( 'NONE',  ( 19.76811771667562567, 17.11192033871618534, 12.25316411605952283 ) ) ;
#11031 = CYLINDRICAL_SURFACE ( 'NONE', #859, 31.10000000000000142 ) ;
#11032 = AXIS2_PLACEMENT_3D ( 'NONE', #4914, #2435, #6613 ) ;
#11033 = CARTESIAN_POINT ( 'NONE',  ( 4.000000000000001776, 25.41250000000000142, 11.30940107675849760 ) ) ;
#11034 = CARTESIAN_POINT ( 'NONE',  ( 19.84539375530421168, 19.84539375530412997, 4.662447845253954171 ) ) ;
#11035 = DIRECTION ( 'NONE',  ( 0.000000000000000000, 0.000000000000000000, 1.000000000000000000 ) ) ;
#11036 = ORIENTED_EDGE ( 'NONE', *, *, #10046, .T. ) ;
#11037 = CARTESIAN_POINT ( 'NONE',  ( -3.999999999999998224, 26.96874999877097068, 8.999999999999992895 ) ) ;
#11038 = CARTESIAN_POINT ( 'NONE',  ( -3.756430356250002323, -26.90312499938548285, 11.16877607737301403 ) ) ;
#11039 = CARTESIAN_POINT ( 'NONE',  ( -1.499999999999998224, -10.49999999999999289, 30.00000000000000355 ) ) ;
#11040 = CARTESIAN_POINT ( 'NONE',  ( 1.878215178125004048, 27.12812499938548783, 5.746835883940462963 ) ) ;
#11041 = CARTESIAN_POINT ( 'NONE',  ( 1.500000000000001776, -10.49999999999999289, 25.00000000000000000 ) ) ;
#11043 = EDGE_LOOP ( 'NONE', ( #12636, #22326, #25270, #5759 ) ) ;
#11042 = CARTESIAN_POINT ( 'NONE',  ( 1.878215178125003382, 29.67812499938549209, 12.25316411605952283 ) ) ;
#11044 = ORIENTED_EDGE ( 'NONE', *, *, #24557, .T. ) ;
#11045 = DIRECTION ( 'NONE',  ( 0.000000000000000000, -1.000000000000000000, 0.000000000000000000 ) ) ;
#11046 = ADVANCED_FACE ( 'NONE', ( #16578 ), #20754, .F. ) ;
#11047 = CARTESIAN_POINT ( 'NONE',  ( 19.46753356867312235, 19.46753356867304063, 12.99999999999999112 ) ) ;
#11048 = VERTEX_POINT ( 'NONE', #16460 ) ;
#11049 = CARTESIAN_POINT ( 'NONE',  ( -3.756430356250003655, -28.40312499938548640, 8.999999999999992895 ) ) ;
#11050 = DIRECTION ( 'NONE',  ( 0.000000000000000000, 1.000000000000000000, 0.000000000000000000 ) ) ;
#11051 = CARTESIAN_POINT ( 'NONE',  ( 4.006172263299091013E-15, 25.25312499938549138, 4.662447845253954171 ) ) ;
#11052 = EDGE_CURVE ( 'NONE', #20454, #21926, #14675, .T. ) ;
#11053 = DIRECTION ( 'NONE',  ( -0.000000000000000000, -1.000000000000000000, -0.000000000000000000 ) ) ;
#11054 = CARTESIAN_POINT ( 'NONE',  ( -3.756430356249994773, 28.96562499938548640, 8.999999999999992895 ) ) ;
#11055 = ADVANCED_FACE ( 'NONE', ( #6622 ), #20626, .T. ) ;
#11056 =( BOUNDED_CURVE ( )  B_SPLINE_CURVE ( 2, ( #16442, #2423, #6357, #18148, #14209, #220, #22310, #16168, #20332 ),
 .UNSPECIFIED., .F., .F. ) 
 B_SPLINE_CURVE_WITH_KNOTS ( ( 3, 2, 2, 2, 3 ),
 ( 0.5250000000000000222, 0.5333333333333333259, 0.5500000000000000444, 0.5666666666666666519, 0.5750000000000000666 ),
 .UNSPECIFIED. ) 
 CURVE ( )  GEOMETRIC_REPRESENTATION_ITEM ( )  RATIONAL_B_SPLINE_CURVE ( ( 0.9330127018922194093, 0.9330127018922194093, 1.000000000000000000, 0.8660254037844387076, 1.000000000000000000, 0.8660254037844387076, 1.000000000000000000, 0.9330127018922189652, 0.9330127018922194093 ) ) 
 REPRESENTATION_ITEM ( '' )  );
#11057 = CARTESIAN_POINT ( 'NONE',  ( 4.000000000000003553, 25.45000000000000639, 8.999999999999992895 ) ) ;
#11058 = APPLICATION_PROTOCOL_DEFINITION ( 'draft international standard', 'automotive_design', 1998, #17969 ) ;
#11059 = EDGE_CURVE ( 'NONE', #25112, #2876, #22977, .T. ) ;
#11060 = LINE ( 'NONE', #5055, #10409 ) ;
#11061 = DIRECTION ( 'NONE',  ( 0.000000000000000000, 0.000000000000000000, 1.000000000000000000 ) ) ;
#11062 = CARTESIAN_POINT ( 'NONE',  ( -3.756430356249996994, 25.81562499938548427, 8.999999999999992895 ) ) ;
#11063 = CARTESIAN_POINT ( 'NONE',  ( 4.393401135980992578, 30.78811501957144969, 1.000000000000000000 ) ) ;
#11064 = CARTESIAN_POINT ( 'NONE',  ( 15.30002297792396071, 20.95687722741627468, 6.690598923241487306 ) ) ;
#11065 = CARTESIAN_POINT ( 'NONE',  ( 22.28712185865447637, 19.45869473390820659, 5.535898384862238508 ) ) ;
#11066 = LINE ( 'NONE', #1401, #23854 ) ;
#11067 = CARTESIAN_POINT ( 'NONE',  ( 1.878215178125000939, 27.31562499938548427, 12.25316411605952283 ) ) ;
#11068 = DIRECTION ( 'NONE',  ( 0.000000000000000000, 0.000000000000000000, 1.000000000000000000 ) ) ;
#11069 = CARTESIAN_POINT ( 'NONE',  ( 15.94292067550354730, 21.25531543142222901, 11.16877607737301048 ) ) ;
#11070 = DIRECTION ( 'NONE',  ( 0.000000000000000000, 0.000000000000000000, 1.000000000000000000 ) ) ;
#11071 = ORIENTED_EDGE ( 'NONE', *, *, #14865, .T. ) ;
#11072 = LINE ( 'NONE', #14491, #12183 ) ;
#11073 = CARTESIAN_POINT ( 'NONE',  ( 4.000000000000003553, 28.58124999877096784, 6.690598923241489970 ) ) ;
#11074 = CARTESIAN_POINT ( 'NONE',  ( -2.000000000000000888, -25.37500000000000000, 12.46410161513774817 ) ) ;
#11076 = ORIENTED_EDGE ( 'NONE', *, *, #20753, .F. ) ;
#11075 = LINE ( 'NONE', #15270, #14617 ) ;
#11077 = CARTESIAN_POINT ( 'NONE',  ( -3.756430356249997438, 25.51562499938548356, 11.16877607737301048 ) ) ;
#11078 = VERTEX_POINT ( 'NONE', #1012 ) ;
#11079 = CARTESIAN_POINT ( 'NONE',  ( 1.878215178124995832, -27.99062499938548143, 5.746835883940462963 ) ) ;
#11080 = ORIENTED_EDGE ( 'NONE', *, *, #24826, .F. ) ;
#11081 = ORIENTED_EDGE ( 'NONE', *, *, #10001, .T. ) ;
#11082 = CARTESIAN_POINT ( 'NONE',  ( 19.41783949975652845, 22.86907598272403419, 12.17998752022640474 ) ) ;
#11083 = CARTESIAN_POINT ( 'NONE',  ( 1.878215178124999829, 26.97812499938549280, 12.25316411605952283 ) ) ;
#11084 = ADVANCED_FACE ( 'NONE', ( #2446 ), #24933, .T. ) ;
#11085 = CARTESIAN_POINT ( 'NONE',  ( 2.672651547586948120E-15, -13.33755215474603162, 0.9281249993854823188 ) ) ;
#11086 = EDGE_CURVE ( 'NONE', #23657, #9327, #14612, .T. ) ;
#11087 = CARTESIAN_POINT ( 'NONE',  ( 0.000000000000000000, 0.000000000000000000, -6.500000000000000000 ) ) ;
#11088 = FILL_AREA_STYLE_COLOUR ( '', #3496 ) ;
#11089 = EDGE_CURVE ( 'NONE', #25532, #5321, #18840, .T. ) ;
#11090 = CARTESIAN_POINT ( 'NONE',  ( 0.000000000000000000, 0.000000000000000000, 1.000000000000000000 ) ) ;
#11091 = CARTESIAN_POINT ( 'NONE',  ( -1.878215178124995832, 29.34062499938548285, 5.746835883940462963 ) ) ;
#11092 = EDGE_CURVE ( 'NONE', #7736, #24890, #22451, .T. ) ;
#11093 = CARTESIAN_POINT ( 'NONE',  ( -30.78811501957148167, -4.393401135980793626, 1.000000000000000000 ) ) ;
#11094 = DIRECTION ( 'NONE',  ( 1.000000000000000000, 0.000000000000000000, 0.000000000000000000 ) ) ;
#11095 = AXIS2_PLACEMENT_3D ( 'NONE', #10628, #13097, #2530 ) ;
#11096 = CARTESIAN_POINT ( 'NONE',  ( -3.756430356249996994, 28.06562499938548427, 8.999999999999992895 ) ) ;
#11097 = CARTESIAN_POINT ( 'NONE',  ( -1.859271017917182139E-15, -25.78750000000000142, 12.99999999999999289 ) ) ;
#11098 = LINE ( 'NONE', #23254, #17072 ) ;
#11099 = DIRECTION ( 'NONE',  ( 0.000000000000000000, 0.000000000000000000, 1.000000000000000000 ) ) ;
#11100 = DIRECTION ( 'NONE',  ( 0.000000000000000000, 0.000000000000000000, 1.000000000000000000 ) ) ;
#11101 = CARTESIAN_POINT ( 'NONE',  ( -1.878215178125000939, -26.07812499938548356, 12.25316411605952283 ) ) ;
#11102 = CARTESIAN_POINT ( 'NONE',  ( 0.000000000000000000, 0.000000000000000000, 1.000000000000000000 ) ) ;
#11103 = CARTESIAN_POINT ( 'NONE',  ( 1.071796769724495668, 27.55134618820330061, 12.99999999999999112 ) ) ;
#11104 = CYLINDRICAL_SURFACE ( 'NONE', #17087, 0.5000000000000004441 ) ;
#11105 = CARTESIAN_POINT ( 'NONE',  ( -1.071796769724487675, -28.69240381056766509, 4.999999999999988454 ) ) ;
#11106 = ORIENTED_EDGE ( 'NONE', *, *, #15128, .F. ) ;
#11107 = DIRECTION ( 'NONE',  ( -1.000000000000000000, 0.000000000000000000, -0.000000000000000000 ) ) ;
#11109 = ORIENTED_EDGE ( 'NONE', *, *, #19844, .F. ) ;
#11108 = CARTESIAN_POINT ( 'NONE',  ( 25.16042852506090810, 18.28012134629586072, -6.500000000000000000 ) ) ;
#11110 = ORIENTED_EDGE ( 'NONE', *, *, #23832, .T. ) ;
#11111 = VERTEX_POINT ( 'NONE', #22593 ) ;
#11112 = ORIENTED_EDGE ( 'NONE', *, *, #330, .T. ) ;
#11113 = ORIENTED_EDGE ( 'NONE', *, *, #5301, .T. ) ;
#11114 = FACE_OUTER_BOUND ( 'NONE', #17939, .T. ) ;
#11115 = DIRECTION ( 'NONE',  ( 0.000000000000000000, 0.000000000000000000, 1.000000000000000000 ) ) ;
#11116 = CARTESIAN_POINT ( 'NONE',  ( -3.756430356249996105, 29.04062499938548569, 6.831223922626973533 ) ) ;
#11117 = EDGE_CURVE ( 'NONE', #6515, #10327, #5057, .T. ) ;
#11118 = CARTESIAN_POINT ( 'NONE',  ( -1.878215178124998497, -12.25316411605951927, 1.340624999385482630 ) ) ;
#11119 = CARTESIAN_POINT ( 'NONE',  ( -3.999999999999996003, -6.690598923241487306, 1.481249998770963083 ) ) ;
#11120 = CARTESIAN_POINT ( 'NONE',  ( 1.859271017917182139E-15, 29.38749999999999929, 12.99999999999999289 ) ) ;
#11121 = CARTESIAN_POINT ( 'NONE',  ( 2.672651547586948120E-15, 25.59062499938548640, 13.33755215474602984 ) ) ;
#11122 = EDGE_CURVE ( 'NONE', #3398, #17170, #18406, .T. ) ;
#11123 = CARTESIAN_POINT ( 'NONE',  ( 25.16843286583315020, -6.741346781237215424, 20.00001200000000168 ) ) ;
#11124 = LINE ( 'NONE', #9930, #10107 ) ;
#11125 = CARTESIAN_POINT ( 'NONE',  ( 4.000000000000003553, -6.690598923241489970, 0.4874999999999966582 ) ) ;
#11126 = CARTESIAN_POINT ( 'NONE',  ( 21.21320343559646915, 21.21320343559638744, 8.999999999999992895 ) ) ;
#11127 = LINE ( 'NONE', #19486, #7858 ) ;
#11128 = DIRECTION ( 'NONE',  ( 0.000000000000000000, 0.000000000000000000, 1.000000000000000000 ) ) ;
#11129 = DIRECTION ( 'NONE',  ( -0.000000000000000000, -0.000000000000000000, -1.000000000000000000 ) ) ;
#11130 = DIRECTION ( 'NONE',  ( 0.000000000000000000, 0.000000000000000000, 1.000000000000000000 ) ) ;
#11131 = CARTESIAN_POINT ( 'NONE',  ( -12.74173596767339767, 28.14012133169338270, 1.000000000000000000 ) ) ;
#11132 = CARTESIAN_POINT ( 'NONE',  ( -1.071796769724494336, -25.35759618943234628, 12.99999999999999467 ) ) ;
#11133 = VERTEX_POINT ( 'NONE', #10800 ) ;
#11134 = ORIENTED_EDGE ( 'NONE', *, *, #782, .F. ) ;
#11135 = ORIENTED_EDGE ( 'NONE', *, *, #10714, .T. ) ;
#11136 = CARTESIAN_POINT ( 'NONE',  ( 3.756430356250004987, 25.14062499938548356, 8.999999999999992895 ) ) ;
#11137 = ORIENTED_EDGE ( 'NONE', *, *, #10309, .F. ) ;
#11138 = CARTESIAN_POINT ( 'NONE',  ( -2.672651547586948120E-15, -26.49062499938548143, 13.33755215474602984 ) ) ;
#11139 = ORIENTED_EDGE ( 'NONE', *, *, #16990, .F. ) ;
#11140 = DIRECTION ( 'NONE',  ( -0.000000000000000000, -1.000000000000000000, 0.000000000000000000 ) ) ;
#11141 = ORIENTED_EDGE ( 'NONE', *, *, #6265, .T. ) ;
#11142 = CARTESIAN_POINT ( 'NONE',  ( 22.32573188046904633, -21.65113613650351709, -6.500000000000000000 ) ) ;
#11143 = CARTESIAN_POINT ( 'NONE',  ( 4.000000000000003553, 25.90000000000000213, 8.999999999999992895 ) ) ;
#11144 = CARTESIAN_POINT ( 'NONE',  ( -3.897863563850083146, -30.85476721088024021, -6.500000000000000000 ) ) ;
#11145 = CARTESIAN_POINT ( 'NONE',  ( -1.071796769724488563, 26.66740381056766651, 12.99999999999999289 ) ) ;
#11146 = LINE ( 'NONE', #25161, #4570 ) ;
#11147 = CARTESIAN_POINT ( 'NONE',  ( 16.63234978716043244, 21.94474454307910705, 8.999999999999992895 ) ) ;
#11148 = EDGE_CURVE ( 'NONE', #13117, #3186, #20069, .T. ) ;
#11149 = CARTESIAN_POINT ( 'NONE',  ( 1.859271017917182139E-15, 28.48749999999999716, 12.99999999999999289 ) ) ;
#11150 = CARTESIAN_POINT ( 'NONE',  ( 2.620986760973688460E-15, 26.23750000000000071, 13.61880215351699874 ) ) ;
#11151 = EDGE_CURVE ( 'NONE', #15884, #1343, #23027, .T. ) ;
#11152 = CARTESIAN_POINT ( 'NONE',  ( 20.19238178538755690, 17.53618440742811302, 5.746835883940462963 ) ) ;
#11153 = CARTESIAN_POINT ( 'NONE',  ( 4.000000000000001776, 26.70624999877097139, 11.30940107675849760 ) ) ;
#11154 = ORIENTED_EDGE ( 'NONE', *, *, #7530, .F. ) ;
#11155 = ORIENTED_EDGE ( 'NONE', *, *, #13459, .T. ) ;
#11156 = CARTESIAN_POINT ( 'NONE',  ( 0.000000000000000000, 26.63124999877097565, 13.61880215351699874 ) ) ;
#11157 = DIRECTION ( 'NONE',  ( -0.000000000000000000, 0.000000000000000000, 1.000000000000000000 ) ) ;
#11158 = ADVANCED_FACE ( 'NONE', ( #14874 ), #880, .F. ) ;
#11159 = CARTESIAN_POINT ( 'NONE',  ( 0.5000000000000000000, -0.8660254037844387076, 19.50000000000000000 ) ) ;
#11160 = CARTESIAN_POINT ( 'NONE',  ( 3.756430356250003655, 27.05312499938548498, 8.999999999999992895 ) ) ;
#11161 = CARTESIAN_POINT ( 'NONE',  ( 4.393401135981119587, 30.78811501957143193, -2.750000000000000000 ) ) ;
#11162 = ORIENTED_EDGE ( 'NONE', *, *, #14205, .T. ) ;
#11163 = ORIENTED_EDGE ( 'NONE', *, *, #24238, .T. ) ;
#11164 = CARTESIAN_POINT ( 'NONE',  ( 5.706339097770919189, 31.50000000000000000, 7.645898033750285983 ) ) ;
#11165 = VECTOR ( 'NONE', #15868, 1000.000000000000000 ) ;
#11166 = CARTESIAN_POINT ( 'NONE',  ( -13.69242354489172797, -27.92360179968362743, -2.750000000000000000 ) ) ;
#11167 = ORIENTED_EDGE ( 'NONE', *, *, #10282, .T. ) ;
#11168 = CARTESIAN_POINT ( 'NONE',  ( 3.756430356249997438, -28.21562499938548640, 11.16877607737301048 ) ) ;
#11169 = CARTESIAN_POINT ( 'NONE',  ( 3.756430356250003211, 29.19062499938548072, 8.999999999999992895 ) ) ;
#11170 = CARTESIAN_POINT ( 'NONE',  ( 3.756430356250004099, 26.00312499938548783, 11.16877607737301403 ) ) ;
#11171 = DIRECTION ( 'NONE',  ( 0.000000000000000000, 0.000000000000000000, 1.000000000000000000 ) ) ;
#11172 = CARTESIAN_POINT ( 'NONE',  ( -1.999999999999996669, 25.15000000000000568, 5.535898384862237620 ) ) ;
#11173 = CARTESIAN_POINT ( 'NONE',  ( 2.000000000000000000, 28.91874999877097707, 12.46410161513774817 ) ) ;
#11174 = SHAPE_DEFINITION_REPRESENTATION ( #8398, #8162 ) ;
#11175 = DIRECTION ( 'NONE',  ( -0.7071067811865487940, -0.7071067811865463515, 0.000000000000000000 ) ) ;
#11176 = CARTESIAN_POINT ( 'NONE',  ( 0.000000000000000000, 0.000000000000000000, -6.500000000000000000 ) ) ;
#11177 = EDGE_CURVE ( 'NONE', #1111, #1657, #20610, .T. ) ;
#11178 = AXIS2_PLACEMENT_3D ( 'NONE', #25381, #13621, #7849 ) ;
#11179 = CARTESIAN_POINT ( 'NONE',  ( 2.672651547586948120E-15, 27.72812499938548569, 13.33755215474603162 ) ) ;
#11180 = CARTESIAN_POINT ( 'NONE',  ( -3.182002658620821212, -29.83112730774910659, 6.562149109989046103 ) ) ;
#11181 = CARTESIAN_POINT ( 'NONE',  ( 19.67524618651571799, 16.84681906176946242, 12.46410161513774817 ) ) ;
#11182 = CARTESIAN_POINT ( 'NONE',  ( 21.05852382634284936, 21.05852382634278186, 13.61880215351699874 ) ) ;
#11183 = CARTESIAN_POINT ( 'NONE',  ( 18.24657187926979063, 19.76232140712176744, 4.999999999999992895 ) ) ;
#11184 = CARTESIAN_POINT ( 'NONE',  ( -3.756430356249996994, 27.16562499938548214, 8.999999999999992895 ) ) ;
#11186 = EDGE_CURVE ( 'NONE', #855, #25560, #11731, .T. ) ;
#11185 = CARTESIAN_POINT ( 'NONE',  ( -22.17092431280609333, -21.28941499438201745, -6.500000000000000000 ) ) ;
#11187 = CARTESIAN_POINT ( 'NONE',  ( 18.46426205773553164, 21.12045943569482986, 5.746835883940462963 ) ) ;
#11188 = CARTESIAN_POINT ( 'NONE',  ( 20.89942480057588980, 20.89942480057579033, 4.999999999999992006 ) ) ;
#11189 = AXIS2_PLACEMENT_3D ( 'NONE', #16217, #19615, #23939 ) ;
#11190 = EDGE_LOOP ( 'NONE', ( #11681, #15944, #5389, #25681 ) ) ;
#11191 = DIRECTION ( 'NONE',  ( -0.9297764858882481276, 0.3681245526846864125, 0.000000000000000000 ) ) ;
#11192 = CARTESIAN_POINT ( 'NONE',  ( 3.756430356250004099, 25.29062499938548569, 6.831223922626973533 ) ) ;
#11193 = CARTESIAN_POINT ( 'NONE',  ( 3.756430356249997882, -29.45312499938548356, 11.16877607737301226 ) ) ;
#11195 = ORIENTED_EDGE ( 'NONE', *, *, #20514, .F. ) ;
#11194 = CARTESIAN_POINT ( 'NONE',  ( 0.000000000000000000, 0.000000000000000000, -6.500000000000000000 ) ) ;
#11196 = CARTESIAN_POINT ( 'NONE',  ( 3.735045420075836212E-15, 25.36562499938548854, 4.662447845253954171 ) ) ;
#11197 = ORIENTED_EDGE ( 'NONE', *, *, #16724, .T. ) ;
#11198 = CARTESIAN_POINT ( 'NONE',  ( 3.756430356249995661, -27.57812499938548356, 6.831223922626973533 ) ) ;
#11199 = ORIENTED_EDGE ( 'NONE', *, *, #14074, .F. ) ;
#11200 = EDGE_CURVE ( 'NONE', #17840, #14500, #21522, .T. ) ;
#11201 = ORIENTED_EDGE ( 'NONE', *, *, #11664, .F. ) ;
#11202 = CARTESIAN_POINT ( 'NONE',  ( 20.83838200801861973, 21.58304260418841380, 12.97381592328244082 ) ) ;
#11203 = CARTESIAN_POINT ( 'NONE',  ( 3.756430356250004987, 26.60312499938548569, 8.999999999999992895 ) ) ;
#11204 = VECTOR ( 'NONE', #3247, 1000.000000000000000 ) ;
#11205 = VECTOR ( 'NONE', #20749, 1000.000000000000000 ) ;
#11206 = CARTESIAN_POINT ( 'NONE',  ( -1.878215178124998497, -12.25316411605951927, 1.790624999385481697 ) ) ;
#11207 = CIRCLE ( 'NONE', #19147, 0.4999999999999998890 ) ;
#11208 = VECTOR ( 'NONE', #22876, 1000.000000000000000 ) ;
#11209 = CARTESIAN_POINT ( 'NONE',  ( 3.735045420075836212E-15, -4.662447845253954171, 3.515624999385486227 ) ) ;
#11210 = EDGE_CURVE ( 'NONE', #17608, #585, #17233, .T. ) ;
#11211 = LINE ( 'NONE', #25226, #16795 ) ;
#11212 = CYLINDRICAL_SURFACE ( 'NONE', #4632, 1.000000000000000000 ) ;
#11213 = LINE ( 'NONE', #17379, #23028 ) ;
#11214 = CARTESIAN_POINT ( 'NONE',  ( -1.878215178124998497, 28.14062499938548356, 12.25316411605951927 ) ) ;
#11215 = DIRECTION ( 'NONE',  ( 0.000000000000000000, 0.000000000000000000, 1.000000000000000000 ) ) ;
#11216 = FACE_OUTER_BOUND ( 'NONE', #16165, .T. ) ;
#11217 = DIRECTION ( 'NONE',  ( -0.000000000000000000, -0.000000000000000000, 1.000000000000000000 ) ) ;
#11218 = CARTESIAN_POINT ( 'NONE',  ( 0.000000000000000000, 0.000000000000000000, 19.00000000000000000 ) ) ;
#11219 = CARTESIAN_POINT ( 'NONE',  ( -3.756430356250002323, -29.26562499938548356, 11.16877607737301226 ) ) ;
#11220 = CARTESIAN_POINT ( 'NONE',  ( -3.756430356249996994, 25.92812499938548498, 8.999999999999992895 ) ) ;
#11222 = ADVANCED_FACE ( 'NONE', ( #19044 ), #9245, .F. ) ;
#11221 = DIRECTION ( 'NONE',  ( -0.000000000000000000, -0.000000000000000000, 1.000000000000000000 ) ) ;
#11223 = AXIS2_PLACEMENT_3D ( 'NONE', #6082, #211, #15903 ) ;
#11224 = CARTESIAN_POINT ( 'NONE',  ( 2.620986760973688460E-15, -13.61880215351699874, 4.387499999999998401 ) ) ;
#11225 = CARTESIAN_POINT ( 'NONE',  ( -5.532151103383257329, 31.50000000000000000, 6.677220593914390712 ) ) ;
#11226 = ORIENTED_EDGE ( 'NONE', *, *, #21962, .T. ) ;
#11227 = CARTESIAN_POINT ( 'NONE',  ( 3.756430356250004543, 29.71562499938548996, 11.16877607737301226 ) ) ;
#11228 = LINE ( 'NONE', #13335, #2926 ) ;
#11230 = ORIENTED_EDGE ( 'NONE', *, *, #6520, .T. ) ;
#11229 = DIRECTION ( 'NONE',  ( 1.000000000000000000, 0.000000000000000000, -0.000000000000000000 ) ) ;
#11231 = EDGE_CURVE ( 'NONE', #6673, #13859, #11066, .T. ) ;
#11232 = VECTOR ( 'NONE', #4651, 1000.000000000000000 ) ;
#11233 = ORIENTED_EDGE ( 'NONE', *, *, #2161, .F. ) ;
#11235 = ORIENTED_EDGE ( 'NONE', *, *, #14804, .T. ) ;
#11234 = AXIS2_PLACEMENT_3D ( 'NONE', #1302, #15179, #25238 ) ;
#11236 = ORIENTED_EDGE ( 'NONE', *, *, #13393, .T. ) ;
#11237 = EDGE_CURVE ( 'NONE', #14695, #22241, #23279, .T. ) ;
#11238 = VERTEX_POINT ( 'NONE', #19428 ) ;
#11239 = DIRECTION ( 'NONE',  ( -0.7071067811865487940, -0.7071067811865463515, 0.000000000000000000 ) ) ;
#11240 = DIRECTION ( 'NONE',  ( 0.000000000000000000, 0.000000000000000000, 1.000000000000000000 ) ) ;
#11241 = DIRECTION ( 'NONE',  ( -0.000000000000000000, -0.000000000000000000, -1.000000000000000000 ) ) ;
#11242 = AXIS2_PLACEMENT_3D ( 'NONE', #14244, #639, #24163 ) ;
#11243 = CARTESIAN_POINT ( 'NONE',  ( 3.756430356250004099, -6.831223922626973533, 1.528124999385482186 ) ) ;
#11244 = CARTESIAN_POINT ( 'NONE',  ( 3.752267015613588906E-15, -4.381197846482986158, 0.9562499987709653926 ) ) ;
#11245 = CARTESIAN_POINT ( 'NONE',  ( 3.735045420075836212E-15, 26.26562499938548356, 4.662447845253954171 ) ) ;
#11246 = AXIS2_PLACEMENT_3D ( 'NONE', #6195, #463, #10363 ) ;
#11247 = CARTESIAN_POINT ( 'NONE',  ( -31.00322564728516639, -2.451530025008796798, -6.500000000000000000 ) ) ;
#11248 = CARTESIAN_POINT ( 'NONE',  ( 1.626862140677534194E-14, 28.43124999877096570, 12.99999999999999289 ) ) ;
#11249 = CARTESIAN_POINT ( 'NONE',  ( -3.756430356249996994, -8.999999999999992895, 3.515624999385482674 ) ) ;
#11250 = DIRECTION ( 'NONE',  ( 1.000000000000000000, 0.000000000000000000, 0.000000000000000000 ) ) ;
#11251 = CYLINDRICAL_SURFACE ( 'NONE', #16209, 0.5000000000000004441 ) ;
#11252 = CARTESIAN_POINT ( 'NONE',  ( 20.42212772327495784, 20.42212772327488679, 12.99999999999999289 ) ) ;
#11253 = CARTESIAN_POINT ( 'NONE',  ( 1.999999999999995781, -27.79374999877096997, 5.535898384862237620 ) ) ;
#11254 = CARTESIAN_POINT ( 'NONE',  ( -3.999999999999996447, -8.999999999999992895, 0.6187499987709670357 ) ) ;
#11255 = CARTESIAN_POINT ( 'NONE',  ( -2.000000000000000000, 25.30000000000001137, 12.46410161513774639 ) ) ;
#11256 = AXIS2_PLACEMENT_3D ( 'NONE', #14719, #17550, #4779 ) ;
#11257 = DIRECTION ( 'NONE',  ( 0.000000000000000000, 1.000000000000000000, 0.000000000000000000 ) ) ;
#11258 = ORIENTED_EDGE ( 'NONE', *, *, #769, .T. ) ;
#11259 = CARTESIAN_POINT ( 'NONE',  ( -1.071796769724492338, -28.95759618943233704, 12.99999999999999467 ) ) ;
#11260 = EDGE_LOOP ( 'NONE', ( #11162, #20574, #9116, #19117 ) ) ;
#11261 = ORIENTED_EDGE ( 'NONE', *, *, #23187, .F. ) ;
#11262 = CARTESIAN_POINT ( 'NONE',  ( 0.000000000000000000, 0.000000000000000000, 1.000000000000000000 ) ) ;
#11263 = ORIENTED_EDGE ( 'NONE', *, *, #24863, .T. ) ;
#11264 = CARTESIAN_POINT ( 'NONE',  ( -3.756430356250002323, -28.81562499938548427, 11.16877607737301226 ) ) ;
#11265 = EDGE_CURVE ( 'NONE', #14631, #6939, #7989, .T. ) ;
#11266 = ORIENTED_EDGE ( 'NONE', *, *, #6733, .F. ) ;
#11267 = DIRECTION ( 'NONE',  ( 0.000000000000000000, 0.000000000000000000, 1.000000000000000000 ) ) ;
#11269 = EDGE_CURVE ( 'NONE', #10289, #5651, #3603, .T. ) ;
#11268 = VECTOR ( 'NONE', #5053, 1000.000000000000000 ) ;
#11270 = EDGE_LOOP ( 'NONE', ( #18076, #1354, #11110, #20395 ) ) ;
#11271 = CARTESIAN_POINT ( 'NONE',  ( -3.999999999999996447, 26.57500000000000284, 8.999999999999992895 ) ) ;
#11272 = EDGE_CURVE ( 'NONE', #10327, #6515, #22168, .T. ) ;
#11273 = CARTESIAN_POINT ( 'NONE',  ( 0.000000000000000000, 10.00000000000000000, 13.00000000000000178 ) ) ;
#11274 = EDGE_CURVE ( 'NONE', #6423, #17283, #24698, .T. ) ;
#11275 = VECTOR ( 'NONE', #20729, 1000.000000000000000 ) ;
#11276 = DIRECTION ( 'NONE',  ( 1.000000000000000000, 0.000000000000000000, 0.000000000000000000 ) ) ;
#11277 = DIRECTION ( 'NONE',  ( 1.000000000000000000, 0.000000000000000000, 0.000000000000000000 ) ) ;
#11278 = CARTESIAN_POINT ( 'NONE',  ( 20.51057983692150444, 17.85438245896205700, 5.746835883940462963 ) ) ;
#11279 =( BOUNDED_CURVE ( )  B_SPLINE_CURVE ( 2, ( #6176, #16525, #12198, #24485, #22526, #4607, #957, #24752, #13366 ),
 .UNSPECIFIED., .F., .F. ) 
 B_SPLINE_CURVE_WITH_KNOTS ( ( 3, 2, 2, 2, 3 ),
 ( 0.4750000000000000333, 0.4833333333333333370, 0.5000000000000000000, 0.5166666666666667185, 0.5250000000000000222 ),
 .UNSPECIFIED. ) 
 CURVE ( )  GEOMETRIC_REPRESENTATION_ITEM ( )  RATIONAL_B_SPLINE_CURVE ( ( 0.9330127018922194093, 0.9330127018922196314, 1.000000000000000000, 0.8660254037844387076, 1.000000000000000000, 0.8660254037844387076, 1.000000000000000000, 0.9330127018922194093, 0.9330127018922194093 ) ) 
 REPRESENTATION_ITEM ( '' )  );
#11280 = CIRCLE ( 'NONE', #14635, 0.5000000000000006661 ) ;
#11281 = CARTESIAN_POINT ( 'NONE',  ( -30.24338421796775123, 7.248980000274508839, -2.750000000000000000 ) ) ;
#11282 = CIRCLE ( 'NONE', #14636, 1.500000000000000222 ) ;
#11283 = CARTESIAN_POINT ( 'NONE',  ( -1.999999999999995781, 25.15000000000000213, 5.535898384862237620 ) ) ;
#11284 = CLOSED_SHELL ( 'NONE', ( #12038, #9688, #768, #3593, #13380, #10374, #14284, #18654, #13137, #15455, #277, #9471, #20955, #9789, #14218, #18958, #11055, #21598, #12615, #6535, #9128, #13964, #15442, #22657, #20318, #1422, #18176, #3689, #17943, #6556, #22136 ) ) ;
#11285 = AXIS2_PLACEMENT_3D ( 'NONE', #7753, #15132, #5780 ) ;
#11286 = CARTESIAN_POINT ( 'NONE',  ( 15.96943717979804056, 21.28183193571671694, 6.831223922626973533 ) ) ;
#11287 = FACE_OUTER_BOUND ( 'NONE', #6395, .T. ) ;
#11288 = EDGE_LOOP ( 'NONE', ( #17365, #18352, #9185, #20759, #2640, #13627, #13677, #8451, #5002, #13247, #11620, #13539, #8316, #6085, #25246, #19697, #13716, #4198, #15684, #19400, #25302, #6905, #13710, #16681 ) ) ;
#11289 = ORIENTED_EDGE ( 'NONE', *, *, #16237, .F. ) ;
#11290 = CARTESIAN_POINT ( 'NONE',  ( 4.000000000000002665, 26.70624999877097494, 11.30940107675849760 ) ) ;
#11291 = CARTESIAN_POINT ( 'NONE',  ( 1.071796769724498999, 28.05759618943233491, 12.99999999999998757 ) ) ;
#11292 = VERTEX_POINT ( 'NONE', #5440 ) ;
#11293 = DIRECTION ( 'NONE',  ( 0.000000000000000000, 0.000000000000000000, -1.000000000000000000 ) ) ;
#11294 = CIRCLE ( 'NONE', #23418, 31.10000000000000142 ) ;
#11295 = CARTESIAN_POINT ( 'NONE',  ( 1.878215178125004048, 28.47812499938548569, 5.746835883940462963 ) ) ;
#11296 = DIRECTION ( 'NONE',  ( 1.000000000000000000, 0.000000000000000000, 0.000000000000000000 ) ) ;
#11297 = EDGE_LOOP ( 'NONE', ( #5261, #15630, #23950, #9117 ) ) ;
#11298 = ORIENTED_EDGE ( 'NONE', *, *, #12543, .F. ) ;
#11299 = CYLINDRICAL_SURFACE ( 'NONE', #22517, 4.000000000000000000 ) ;
#11300 = CIRCLE ( 'NONE', #15902, 0.4999999999999996114 ) ;
#11301 = ADVANCED_FACE ( 'NONE', ( #3483 ), #1519, .T. ) ;
#11302 = AXIS2_PLACEMENT_3D ( 'NONE', #7041, #4436, #10830 ) ;
#11303 = CARTESIAN_POINT ( 'NONE',  ( -27.92360179968358125, 13.69242354489182922, -6.500000000000000000 ) ) ;
#11304 = EDGE_LOOP ( 'NONE', ( #9086, #15654, #2370, #10204 ) ) ;
#11305 = CIRCLE ( 'NONE', #15458, 0.5000000000000004441 ) ;
#11306 = CARTESIAN_POINT ( 'NONE',  ( -2.672651547586948120E-15, -29.64062499938548356, 13.33755215474603162 ) ) ;
#11307 = CARTESIAN_POINT ( 'NONE',  ( 1.878215178125000939, 25.51562499938548356, 12.25316411605952283 ) ) ;
#11308 = CARTESIAN_POINT ( 'NONE',  ( 3.756430356250006319, 25.17812499938548854, 6.831223922626973533 ) ) ;
#11309 = CIRCLE ( 'NONE', #12150, 0.5000000000000007772 ) ;
#11310 = DIRECTION ( 'NONE',  ( 0.000000000000000000, 0.000000000000000000, -1.000000000000000000 ) ) ;
#11311 = CARTESIAN_POINT ( 'NONE',  ( 3.756430356250004987, 29.64062499938548711, 8.999999999999992895 ) ) ;
#11312 = EDGE_CURVE ( 'NONE', #23396, #23209, #11315, .T. ) ;
#11313 = AXIS2_PLACEMENT_3D ( 'NONE', #7899, #199, #14184 ) ;
#11314 = CARTESIAN_POINT ( 'NONE',  ( 1.580380365229604700E-14, 27.58750000000000213, 12.99999999999999289 ) ) ;
#11315 = CIRCLE ( 'NONE', #22631, 0.4999999999999998335 ) ;
#11316 = VECTOR ( 'NONE', #23383, 999.9999999999998863 ) ;
#11317 = DIRECTION ( 'NONE',  ( 1.000000000000000000, 0.000000000000000000, 0.000000000000000000 ) ) ;
#11318 = CARTESIAN_POINT ( 'NONE',  ( -3.756430356249996105, 25.77812499938548285, 6.831223922626973533 ) ) ;
#11319 = CARTESIAN_POINT ( 'NONE',  ( -26.25859848311247902, 16.66421332384710752, 1.000000000000000000 ) ) ;
#11320 = CARTESIAN_POINT ( 'NONE',  ( 17.79907597611823533, 23.11147073203690283, 6.831223922626973533 ) ) ;
#11321 = CARTESIAN_POINT ( 'NONE',  ( 22.10157009459123856, 19.44537271663178757, 5.746835883940462963 ) ) ;
#11322 = CARTESIAN_POINT ( 'NONE',  ( 19.37161951330217136, 20.88736904115415172, 12.99999999999999289 ) ) ;
#11323 = CARTESIAN_POINT ( 'NONE',  ( -1.878215178124998497, 28.59062499938548285, 12.25316411605951927 ) ) ;
#11324 = VECTOR ( 'NONE', #2025, 1000.000000000000000 ) ;
#11325 = DIRECTION ( 'NONE',  ( 0.000000000000000000, 0.000000000000000000, 1.000000000000000000 ) ) ;
#11326 = CARTESIAN_POINT ( 'NONE',  ( 17.50739442887878639, 22.81978918479745744, 8.999999999999992895 ) ) ;
#11327 = CARTESIAN_POINT ( 'NONE',  ( 20.55781653595669667, 19.04206700810457065, 12.99999999999998757 ) ) ;
#11328 = ORIENTED_EDGE ( 'NONE', *, *, #16240, .F. ) ;
#11329 = CARTESIAN_POINT ( 'NONE',  ( 2.000000000000003997, 26.81874999877096855, 5.535898384862238508 ) ) ;
#11330 = CARTESIAN_POINT ( 'NONE',  ( 4.000000000000003553, 29.48124999877096997, 6.690598923241489970 ) ) ;
#11331 = CARTESIAN_POINT ( 'NONE',  ( -4.000000000000003553, -25.03749999999999787, 6.690598923241489970 ) ) ;
#11333 = ORIENTED_EDGE ( 'NONE', *, *, #23220, .T. ) ;
#11332 = LINE ( 'NONE', #11848, #20371 ) ;
#11334 = CARTESIAN_POINT ( 'NONE',  ( 3.756430356250003655, 25.70312499938548356, 8.999999999999992895 ) ) ;
#11335 = CIRCLE ( 'NONE', #18467, 31.10000000000000142 ) ;
#11336 = CARTESIAN_POINT ( 'NONE',  ( 26.00000000000000711, 1.701696020694481559, 20.00001200000000523 ) ) ;
#11337 = CARTESIAN_POINT ( 'NONE',  ( -3.756430356250002323, -27.80312499938548143, 11.16877607737301226 ) ) ;
#11338 = EDGE_LOOP ( 'NONE', ( #255, #9914, #7091, #14950 ) ) ;
#11339 = ORIENTED_EDGE ( 'NONE', *, *, #15078, .T. ) ;
#11340 = DIRECTION ( 'NONE',  ( 0.000000000000000000, 0.000000000000000000, 1.000000000000000000 ) ) ;
#11341 = AXIS2_PLACEMENT_3D ( 'NONE', #21443, #1559, #12848 ) ;
#11342 = CARTESIAN_POINT ( 'NONE',  ( -3.756430356250002323, 27.31562499938548783, 11.16877607737301226 ) ) ;
#11343 = CIRCLE ( 'NONE', #14701, 0.5000000000000003331 ) ;
#11344 = EDGE_CURVE ( 'NONE', #9390, #12699, #5576, .T. ) ;
#11345 = CARTESIAN_POINT ( 'NONE',  ( 1.878215178125004048, -5.746835883940462963, 2.015624999385484450 ) ) ;
#11346 = AXIS2_PLACEMENT_3D ( 'NONE', #22415, #16666, #24775 ) ;
#11347 = DIRECTION ( 'NONE',  ( 0.000000000000000000, 0.000000000000000000, 1.000000000000000000 ) ) ;
#11348 = FILL_AREA_STYLE_COLOUR ( '', #14372 ) ;
#11349 = EDGE_CURVE ( 'NONE', #56, #3531, #4231, .T. ) ;
#11350 = CARTESIAN_POINT ( 'NONE',  ( 3.999999999999995559, -27.38124999877096855, 6.690598923241487306 ) ) ;
#11351 = CARTESIAN_POINT ( 'NONE',  ( 0.000000000000000000, 0.000000000000000000, 1.000000000000000000 ) ) ;
#11352 = CIRCLE ( 'NONE', #10941, 0.7500000000000001110 ) ;
#11353 = DIRECTION ( 'NONE',  ( 0.000000000000000000, 0.000000000000000000, -1.000000000000000000 ) ) ;
#11354 = CARTESIAN_POINT ( 'NONE',  ( -3.959305739469038251E-15, -30.00000000000000355, 12.99999999999999289 ) ) ;
#11355 = FACE_OUTER_BOUND ( 'NONE', #3808, .T. ) ;
#11356 = DIRECTION ( 'NONE',  ( 1.000000000000000000, 0.000000000000000000, 0.000000000000000000 ) ) ;
#11357 = FACE_OUTER_BOUND ( 'NONE', #23816, .T. ) ;
#11358 = ORIENTED_EDGE ( 'NONE', *, *, #14332, .F. ) ;
#11359 = CARTESIAN_POINT ( 'NONE',  ( 18.28012134629577190, -25.16042852506097205, -6.500000000000000000 ) ) ;
#11360 = CARTESIAN_POINT ( 'NONE',  ( 1.878215178124995832, -29.45312499938548356, 5.746835883940462963 ) ) ;
#11361 = CIRCLE ( 'NONE', #17646, 31.10000000000000142 ) ;
#11362 = CARTESIAN_POINT ( 'NONE',  ( -3.756430356250003655, -25.14062499938548356, 8.999999999999992895 ) ) ;
#11363 = LINE ( 'NONE', #15560, #1218 ) ;
#11364 = DIRECTION ( 'NONE',  ( 0.000000000000000000, 0.000000000000000000, -1.000000000000000000 ) ) ;
#11365 = ORIENTED_EDGE ( 'NONE', *, *, #3416, .F. ) ;
#11366 = CARTESIAN_POINT ( 'NONE',  ( 3.756430356250004543, 29.34062499938548640, 6.831223922626973533 ) ) ;
#11367 = AXIS2_PLACEMENT_3D ( 'NONE', #16830, #6876, #22958 ) ;
#11368 = CARTESIAN_POINT ( 'NONE',  ( -0.7500000000000000000, 0.000000000000000000, 17.69999999999999929 ) ) ;
#11370 = ORIENTED_EDGE ( 'NONE', *, *, #23269, .F. ) ;
#11369 = DIRECTION ( 'NONE',  ( 1.000000000000000000, 0.000000000000000000, 0.000000000000000000 ) ) ;
#11371 = VECTOR ( 'NONE', #22835, 1000.000000000000000 ) ;
#11372 = ORIENTED_EDGE ( 'NONE', *, *, #3328, .F. ) ;
#11373 = ORIENTED_EDGE ( 'NONE', *, *, #8853, .T. ) ;
#11374 = VERTEX_POINT ( 'NONE', #15766 ) ;
#11375 = VERTEX_POINT ( 'NONE', #2170 ) ;
#11376 = DIRECTION ( 'NONE',  ( 0.000000000000000000, 0.000000000000000000, 1.000000000000000000 ) ) ;
#11377 = FACE_OUTER_BOUND ( 'NONE', #10995, .T. ) ;
#11378 = VECTOR ( 'NONE', #20246, 1000.000000000000000 ) ;
#11379 = EDGE_CURVE ( 'NONE', #7733, #20732, #4410, .T. ) ;
#11380 = DIRECTION ( 'NONE',  ( -0.000000000000000000, -0.000000000000000000, 1.000000000000000000 ) ) ;
#11381 = AXIS2_PLACEMENT_3D ( 'NONE', #12725, #20694, #16784 ) ;
#11382 = EDGE_CURVE ( 'NONE', #5606, #990, #19932, .T. ) ;
#11383 = CARTESIAN_POINT ( 'NONE',  ( 3.756430356250003655, -8.999999999999992895, 2.390624999385481342 ) ) ;
#11384 = CARTESIAN_POINT ( 'NONE',  ( -3.999999999999997335, -11.30940107675849404, 2.456249998770964726 ) ) ;
#11385 =( LENGTH_UNIT ( ) NAMED_UNIT ( * ) SI_UNIT ( .MILLI., .METRE. ) );
#11386 = ADVANCED_FACE ( 'NONE', ( #17857 ), #25705, .F. ) ;
#11387 = CARTESIAN_POINT ( 'NONE',  ( -3.756430356249996994, 27.72812499938548569, 8.999999999999992895 ) ) ;
#11388 = CARTESIAN_POINT ( 'NONE',  ( 4.000000000000003553, 29.73213749463701561, 8.999999999999992895 ) ) ;
#11389 = CARTESIAN_POINT ( 'NONE',  ( 19.61779375967526562, 22.44622088442137908, 12.46410161513774639 ) ) ;
#11390 = CARTESIAN_POINT ( 'NONE',  ( -3.999999999999996003, -6.690598923241487306, 1.087499999999996358 ) ) ;
#11391 = CARTESIAN_POINT ( 'NONE',  ( 4.000000000000003553, -8.999999999999992895, 18.00000000000000000 ) ) ;
#11393 = EDGE_CURVE ( 'NONE', #15245, #2906, #13010, .T. ) ;
#11392 = CYLINDRICAL_SURFACE ( 'NONE', #19956, 0.5000000000000002220 ) ;
#11394 = CARTESIAN_POINT ( 'NONE',  ( 28.34936733434205536, 12.78762572734047254, -6.500000000000000000 ) ) ;
#11395 = CARTESIAN_POINT ( 'NONE',  ( -4.000000000000003553, -26.74374999877096926, 8.999999999999992895 ) ) ;
#11396 = CARTESIAN_POINT ( 'NONE',  ( 3.735045420075836212E-15, -4.662447845253954171, 3.965624999385486404 ) ) ;
#11397 = DIRECTION ( 'NONE',  ( 1.000000000000000000, 0.000000000000000000, 0.000000000000000000 ) ) ;
#11398 = AXIS2_PLACEMENT_3D ( 'NONE', #21767, #19668, #22017 ) ;
#11399 = CARTESIAN_POINT ( 'NONE',  ( -4.000000000000003553, -25.00000000000000000, 8.999999999999992895 ) ) ;
#11400 = CARTESIAN_POINT ( 'NONE',  ( 0.000000000000000000, 0.000000000000000000, 17.00000000000000000 ) ) ;
#11401 = EDGE_LOOP ( 'NONE', ( #11936, #22007, #5257, #20889 ) ) ;
#11402 = DIRECTION ( 'NONE',  ( 1.000000000000000000, 0.000000000000000000, 0.000000000000000000 ) ) ;
#11403 = ORIENTED_EDGE ( 'NONE', *, *, #12397, .T. ) ;
#11404 = CIRCLE ( 'NONE', #14751, 2.000000000000000000 ) ;
#11405 = VERTEX_POINT ( 'NONE', #12228 ) ;
#11406 = DIRECTION ( 'NONE',  ( 0.000000000000000000, 0.000000000000000000, 1.000000000000000000 ) ) ;
#11407 = ORIENTED_EDGE ( 'NONE', *, *, #13065, .F. ) ;
#11408 = CARTESIAN_POINT ( 'NONE',  ( -3.735045420075836212E-15, -28.06562499938548427, 4.662447845253954171 ) ) ;
#11409 = EDGE_LOOP ( 'NONE', ( #11727, #16376, #3555, #2375 ) ) ;
#11410 = CYLINDRICAL_SURFACE ( 'NONE', #25554, 31.10000000000000142 ) ;
#11411 = VECTOR ( 'NONE', #6825, 1000.000000000000000 ) ;
#11412 = ORIENTED_EDGE ( 'NONE', *, *, #9613, .F. ) ;
#11413 = CARTESIAN_POINT ( 'NONE',  ( -1.999999999999995781, 26.50000000000000355, 5.535898384862237620 ) ) ;
#11414 = DIRECTION ( 'NONE',  ( -0.000000000000000000, -1.000000000000000000, -0.000000000000000000 ) ) ;
#11415 = CARTESIAN_POINT ( 'NONE',  ( -30.35476721088030061, -3.897863563849544466, -6.500000000000000000 ) ) ;
#11416 = PRODUCT_RELATED_PRODUCT_CATEGORY ( 'part', '', ( #10050 ) ) ;
#11417 = CARTESIAN_POINT ( 'NONE',  ( 3.834746474454188013E-15, 28.20624999877096428, 4.999999999999992006 ) ) ;
#11418 = CARTESIAN_POINT ( 'NONE',  ( 20.32269083260512588, 20.32269083260505838, 13.33755215474602984 ) ) ;
#11419 = CARTESIAN_POINT ( 'NONE',  ( 16.23990935651698564, -26.52310962334756184, -2.750000000000000000 ) ) ;
#11420 = EDGE_CURVE ( 'NONE', #19518, #25247, #7785, .T. ) ;
#11421 = CARTESIAN_POINT ( 'NONE',  ( 4.000000000000001776, 26.76249999999999929, 11.30940107675849760 ) ) ;
#11422 = ADVANCED_FACE ( 'NONE', ( #6079 ), #20195, .T. ) ;
#11423 = CARTESIAN_POINT ( 'NONE',  ( 19.52719570377026059, 19.52719570377018599, 4.662447845253954171 ) ) ;
#11424 = DIRECTION ( 'NONE',  ( 1.000000000000000000, 0.000000000000000000, 0.000000000000000000 ) ) ;
#11425 = MECHANICAL_DESIGN_GEOMETRIC_PRESENTATION_REPRESENTATION (  '', ( #1825 ), #5588 ) ;
#11426 = ORIENTED_EDGE ( 'NONE', *, *, #10153, .F. ) ;
#11427 = VERTEX_POINT ( 'NONE', #23875 ) ;
#11428 = CARTESIAN_POINT ( 'NONE',  ( -3.999999999999996447, 28.28124999877097778, 6.690598923241487306 ) ) ;
#11429 = DIRECTION ( 'NONE',  ( -0.7071067811865487940, -0.7071067811865463515, 0.000000000000000000 ) ) ;
#11430 = CIRCLE ( 'NONE', #13107, 30.00000000000000355 ) ;
#11431 = ORIENTED_EDGE ( 'NONE', *, *, #22170, .F. ) ;
#11432 = DIRECTION ( 'NONE',  ( 0.000000000000000000, 0.000000000000000000, 1.000000000000000000 ) ) ;
#11433 = CARTESIAN_POINT ( 'NONE',  ( -3.756430356249997882, 28.21562499938548285, 11.16877607737301226 ) ) ;
#11434 = CARTESIAN_POINT ( 'NONE',  ( 17.14423315256455282, 18.65998268041653674, 12.99999999999999467 ) ) ;
#11435 = ORIENTED_EDGE ( 'NONE', *, *, #1682, .F. ) ;
#11436 = EDGE_LOOP ( 'NONE', ( #12363, #3175, #19180, #17179, #8807, #23029, #15493, #20795, #1888, #3050, #5910, #10875, #15906, #21730, #14415, #17806, #17480, #25659, #7507, #2366, #22647, #23196, #10010, #22106 ) ) ;
#11437 =( BOUNDED_CURVE ( )  B_SPLINE_CURVE ( 2, ( #3658, #17534, #25508, #1185, #17672, #5504, #9306, #13225, #13494 ),
 .UNSPECIFIED., .F., .F. ) 
 B_SPLINE_CURVE_WITH_KNOTS ( ( 3, 2, 2, 2, 3 ),
 ( 0.2750000000000000222, 0.2833333333333333259, 0.2999999999999999889, 0.3166666666666666519, 0.3250000000000000111 ),
 .UNSPECIFIED. ) 
 CURVE ( )  GEOMETRIC_REPRESENTATION_ITEM ( )  RATIONAL_B_SPLINE_CURVE ( ( 0.9330127018922194093, 0.9330127018922196314, 1.000000000000000000, 0.8660254037844387076, 1.000000000000000000, 0.8660254037844387076, 1.000000000000000000, 0.9330127018922191873, 0.9330127018922194093 ) ) 
 REPRESENTATION_ITEM ( '' )  );
#11438 = DIRECTION ( 'NONE',  ( 0.000000000000000000, 0.000000000000000000, 1.000000000000000000 ) ) ;
#11439 = ORIENTED_EDGE ( 'NONE', *, *, #12177, .F. ) ;
#11440 = CARTESIAN_POINT ( 'NONE',  ( -3.999999999999995559, 25.63749999999999929, 6.690598923241487306 ) ) ;
#11441 = CARTESIAN_POINT ( 'NONE',  ( -1.878215178124998497, 25.44062499938548427, 12.25316411605951927 ) ) ;
#11442 =( BOUNDED_CURVE ( )  B_SPLINE_CURVE ( 2, ( #404, #2360, #16221, #18311, #22488, #20531, #6147 ),
 .UNSPECIFIED., .F., .F. ) 
 B_SPLINE_CURVE_WITH_KNOTS ( ( 3, 2, 2, 3 ),
 ( 0.6000000000000004219, 0.6166666666666670293, 0.6333333333333336368, 0.6500000000000002442 ),
 .UNSPECIFIED. ) 
 CURVE ( )  GEOMETRIC_REPRESENTATION_ITEM ( )  RATIONAL_B_SPLINE_CURVE ( ( 0.9999999999999964473, 0.8660254037844422603, 1.000000000000000000, 0.8660254037844387076, 1.000000000000000000, 0.8660254037844369313, 1.000000000000001776 ) ) 
 REPRESENTATION_ITEM ( '' )  );
#11443 = CARTESIAN_POINT ( 'NONE',  ( 3.756430356250002323, 27.42812499938548854, 6.831223922626973533 ) ) ;
#11444 = PRESENTATION_LAYER_ASSIGNMENT (  '', '', ( #15619 ) ) ;
#11445 = CARTESIAN_POINT ( 'NONE',  ( 3.469446951953614189E-15, 25.00000000000000000, 8.999999999999992895 ) ) ;
#11446 = CARTESIAN_POINT ( 'NONE',  ( -3.999999999999996447, 26.53750000000000497, 6.690598923241487306 ) ) ;
#11447 = EDGE_CURVE ( 'NONE', #21005, #523, #74, .T. ) ;
#11448 = LINE ( 'NONE', #1393, #2908 ) ;
#11449 = EDGE_CURVE ( 'NONE', #13483, #25775, #2164, .T. ) ;
#11450 = CARTESIAN_POINT ( 'NONE',  ( 0.000000000000000000, 0.000000000000000000, 1.000000000000000000 ) ) ;
#11451 = CARTESIAN_POINT ( 'NONE',  ( -1.878215178124995832, 27.54062499938548214, 5.746835883940462963 ) ) ;
#11452 = CARTESIAN_POINT ( 'NONE',  ( -30.04913349766228592, -5.827558883615738594, -6.500000000000000000 ) ) ;
#11453 = CARTESIAN_POINT ( 'NONE',  ( 22.07057040778514789, 16.41371615829269359, 11.30940107675849760 ) ) ;
#11454 = CARTESIAN_POINT ( 'NONE',  ( 18.54381157061901675, 21.20000894857831852, 5.746835883940462963 ) ) ;
#11455 = DIRECTION ( 'NONE',  ( 0.000000000000000000, 0.000000000000000000, 1.000000000000000000 ) ) ;
#11456 = CARTESIAN_POINT ( 'NONE',  ( 4.000000000000003553, 28.18750000000000000, 6.690598923241489970 ) ) ;
#11457 = CARTESIAN_POINT ( 'NONE',  ( -1.999999999999998224, -12.46410161513774639, 2.943749998770967657 ) ) ;
#11458 = CARTESIAN_POINT ( 'NONE',  ( 15.88988766691455368, 21.20228242283322828, 6.831223922626973533 ) ) ;
#11459 = LINE ( 'NONE', #21526, #22154 ) ;
#11460 = ORIENTED_EDGE ( 'NONE', *, *, #2120, .F. ) ;
#11461 = CARTESIAN_POINT ( 'NONE',  ( 3.752267015613588906E-15, 25.50624999877097565, 4.381197846482986158 ) ) ;
#11462 = CARTESIAN_POINT ( 'NONE',  ( -1.878215178124995832, 26.75312499938548783, 5.746835883940462963 ) ) ;
#11463 = CARTESIAN_POINT ( 'NONE',  ( -4.000000000000001776, -26.31250000000000000, 11.30940107675849760 ) ) ;
#11465 = EDGE_LOOP ( 'NONE', ( #7023, #3953, #22917, #6352 ) ) ;
#11464 = CARTESIAN_POINT ( 'NONE',  ( 4.000000000000001776, 29.46250000000000213, 11.30940107675849760 ) ) ;
#11466 = ADVANCED_FACE ( 'NONE', ( #3867 ), #19928, .F. ) ;
#11467 = CARTESIAN_POINT ( 'NONE',  ( 2.672651547586948120E-15, 25.59062499938548640, 13.33755215474603162 ) ) ;
#11468 = EDGE_CURVE ( 'NONE', #23620, #408, #16039, .T. ) ;
#11469 = CARTESIAN_POINT ( 'NONE',  ( -13.02991752792604707, 22.56362157461192908, 20.00001199999999812 ) ) ;
#11470 = CARTESIAN_POINT ( 'NONE',  ( 3.756430356249995661, -28.92812499938548143, 6.831223922626973533 ) ) ;
#11471 = ORIENTED_EDGE ( 'NONE', *, *, #17833, .F. ) ;
#11472 = VERTEX_POINT ( 'NONE', #4113 ) ;
#11473 = CARTESIAN_POINT ( 'NONE',  ( 18.84476222413640301, 23.34301068176857896, 11.43940974718624659 ) ) ;
#11474 = CARTESIAN_POINT ( 'NONE',  ( 2.003086131649545506E-15, 29.19062499938549138, 13.33755215474602984 ) ) ;
#11475 = CARTESIAN_POINT ( 'NONE',  ( -3.756430356249996994, -8.999999999999992895, 0.3656249993854825409 ) ) ;
#11476 = CARTESIAN_POINT ( 'NONE',  ( 2.672651547586948120E-15, -13.33755215474602984, 4.640624999385483562 ) ) ;
#11477 = SURFACE_STYLE_FILL_AREA ( #5599 ) ;
#11478 = EDGE_CURVE ( 'NONE', #4613, #4306, #12091, .T. ) ;
#11479 = CARTESIAN_POINT ( 'NONE',  ( 29.57785765677924061, -9.610428525060996208, -6.500000000000000000 ) ) ;
#11480 = CARTESIAN_POINT ( 'NONE',  ( 4.000000000000007105, 28.60000000000000497, 8.999999999999992895 ) ) ;
#11481 = DIRECTION ( 'NONE',  ( 1.000000000000000000, 0.000000000000000000, 0.000000000000000000 ) ) ;
#11482 = CARTESIAN_POINT ( 'NONE',  ( 1.071796769724487675, 28.69240381056766509, 4.999999999999988454 ) ) ;
#11483 = DIRECTION ( 'NONE',  ( 0.000000000000000000, 0.000000000000000000, 1.000000000000000000 ) ) ;
#11484 = DIRECTION ( 'NONE',  ( 0.000000000000000000, 0.000000000000000000, 1.000000000000000000 ) ) ;
#11485 = DIRECTION ( 'NONE',  ( -0.2486898871648584586, -0.9685831611286301879, 0.000000000000000000 ) ) ;
#11486 = ORIENTED_EDGE ( 'NONE', *, *, #6278, .T. ) ;
#11487 = CARTESIAN_POINT ( 'NONE',  ( -8.831537335106614961E-15, -27.53124999877097068, 12.99999999999999112 ) ) ;
#11488 = CARTESIAN_POINT ( 'NONE',  ( -3.756430356250002323, -29.71562499938548640, 11.16877607737301226 ) ) ;
#11489 = CARTESIAN_POINT ( 'NONE',  ( 1.878215178125000939, 26.97812499938548569, 12.25316411605952283 ) ) ;
#11490 = EDGE_CURVE ( 'NONE', #1528, #1143, #8179, .T. ) ;
#11491 = DIRECTION ( 'NONE',  ( 0.000000000000000000, 0.000000000000000000, 1.000000000000000000 ) ) ;
#11492 = LINE ( 'NONE', #7435, #5802 ) ;
#11493 = LINE ( 'NONE', #13475, #3471 ) ;
#11494 = ORIENTED_EDGE ( 'NONE', *, *, #2766, .T. ) ;
#11495 = CARTESIAN_POINT ( 'NONE',  ( 6.009258394948636914E-15, 29.41562499938548925, 4.662447845253954171 ) ) ;
#11496 = CARTESIAN_POINT ( 'NONE',  ( -3.897863563849436552, 30.85476721088031482, -6.500000000000000000 ) ) ;
#11498 = ORIENTED_EDGE ( 'NONE', *, *, #422, .F. ) ;
#11497 = CARTESIAN_POINT ( 'NONE',  ( -2.000000000000000888, -26.27499999999999858, 12.46410161513774817 ) ) ;
#11499 = EDGE_CURVE ( 'NONE', #23656, #12264, #17202, .T. ) ;
#11500 = ORIENTED_EDGE ( 'NONE', *, *, #14414, .F. ) ;
#11501 = EDGE_LOOP ( 'NONE', ( #21066, #19735, #14435, #18615 ) ) ;
#11502 = ORIENTED_EDGE ( 'NONE', *, *, #20217, .F. ) ;
#11503 = ORIENTED_EDGE ( 'NONE', *, *, #2543, .F. ) ;
#11504 = FACE_OUTER_BOUND ( 'NONE', #19112, .T. ) ;
#11505 = CARTESIAN_POINT ( 'NONE',  ( -3.295251204612120066, 39.00010698140257404, 13.40411251903217327 ) ) ;
#11506 = CARTESIAN_POINT ( 'NONE',  ( 3.756430356250003211, 25.59062499938548285, 8.999999999999992895 ) ) ;
#11507 = CARTESIAN_POINT ( 'NONE',  ( 3.735045420075836212E-15, -4.662447845253954171, 2.953124999385479565 ) ) ;
#11508 = CARTESIAN_POINT ( 'NONE',  ( -1.999999999999995781, -5.535898384862237620, 2.793749998770966858 ) ) ;
#11509 =( NAMED_UNIT ( * ) PLANE_ANGLE_UNIT ( ) SI_UNIT ( $, .RADIAN. ) );
#11510 =( BOUNDED_CURVE ( )  B_SPLINE_CURVE ( 2, ( #19777, #5534, #7746, #19388, #21737 ),
 .UNSPECIFIED., .F., .F. ) 
 B_SPLINE_CURVE_WITH_KNOTS ( ( 3, 2, 3 ),
 ( 0.9749999999999999778, 0.9833333333333332815, 1.000000000000000000 ),
 .UNSPECIFIED. ) 
 CURVE ( )  GEOMETRIC_REPRESENTATION_ITEM ( )  RATIONAL_B_SPLINE_CURVE ( ( 0.9330127018922194093, 0.9330127018922194093, 1.000000000000000000, 0.8660254037844387076, 1.000000000000000000 ) ) 
 REPRESENTATION_ITEM ( '' )  );
#11511 = CARTESIAN_POINT ( 'NONE',  ( -3.756430356249995661, 27.69062499938548427, 6.831223922626973533 ) ) ;
#11512 = CARTESIAN_POINT ( 'NONE',  ( 0.000000000000000000, 0.000000000000000000, -6.500000000000000000 ) ) ;
#11513 = LINE ( 'NONE', #15707, #2186 ) ;
#11514 = CARTESIAN_POINT ( 'NONE',  ( -3.999999999999996447, -8.999999999999992895, 0.6749999999999984901 ) ) ;
#11515 = CARTESIAN_POINT ( 'NONE',  ( 1.500000000000001776, -7.499999999999993783, 30.00000000000000355 ) ) ;
#11516 = FACE_OUTER_BOUND ( 'NONE', #22679, .T. ) ;
#11517 = CARTESIAN_POINT ( 'NONE',  ( -27.10000000000000142, 0.000000000000000000, 1.000000000000000000 ) ) ;
#11518 = CARTESIAN_POINT ( 'NONE',  ( -3.752267015613588906E-15, -26.85624999877096641, 4.381197846482986158 ) ) ;
#11519 = DIRECTION ( 'NONE',  ( 1.000000000000000000, 0.000000000000000000, 0.000000000000000000 ) ) ;
#11520 = CARTESIAN_POINT ( 'NONE',  ( -25.45105997952931176, -17.87326343783925608, 1.000000000000000000 ) ) ;
#11521 = EDGE_CURVE ( 'NONE', #8734, #15394, #13588, .T. ) ;
#11522 = CARTESIAN_POINT ( 'NONE',  ( -3.999999999999996447, -8.999999999999992895, 4.668749998770968190 ) ) ;
#11523 = CARTESIAN_POINT ( 'NONE',  ( -3.999999999999996447, 25.67500000000000071, 8.999999999999992895 ) ) ;
#11524 = VERTEX_POINT ( 'NONE', #10370 ) ;
#11525 = DIRECTION ( 'NONE',  ( -0.000000000000000000, -0.000000000000000000, 1.000000000000000000 ) ) ;
#11526 = ORIENTED_EDGE ( 'NONE', *, *, #20988, .T. ) ;
#11527 = ADVANCED_FACE ( 'NONE', ( #22418 ), #4638, .F. ) ;
#11528 = EDGE_LOOP ( 'NONE', ( #24469, #13562, #15601, #25845 ) ) ;
#11529 = DIRECTION ( 'NONE',  ( -0.000000000000000000, -0.000000000000000000, 1.000000000000000000 ) ) ;
#11530 = ORIENTED_EDGE ( 'NONE', *, *, #170, .F. ) ;
#11531 = CARTESIAN_POINT ( 'NONE',  ( -2.672651547586948120E-15, -28.74062499938548498, 13.33755215474602984 ) ) ;
#11532 = ORIENTED_EDGE ( 'NONE', *, *, #6632, .T. ) ;
#11533 = FACE_OUTER_BOUND ( 'NONE', #25687, .T. ) ;
#11534 = EDGE_LOOP ( 'NONE', ( #4384, #20967, #12429, #21801 ) ) ;
#11535 = EDGE_CURVE ( 'NONE', #9331, #12074, #2800, .T. ) ;
#11536 = CARTESIAN_POINT ( 'NONE',  ( -3.999999999999997335, 27.06250000000000000, 11.30940107675849404 ) ) ;
#11537 = LINE ( 'NONE', #23577, #17272 ) ;
#11538 = CARTESIAN_POINT ( 'NONE',  ( -3.756430356249997882, -11.16877607737301226, 0.9656249993854834068 ) ) ;
#11539 = B_SPLINE_CURVE_WITH_KNOTS ( 'NONE', 3,
 ( #11607, #19581, #17643, #10285, #24032, #17890, #119, #11989, #15938, #23910, #22062, #13842, #22328, #14233, #25863, #9786, #7818, #6378 ),
 .UNSPECIFIED., .F., .F.,
 ( 4, 2, 2, 2, 2, 2, 2, 2, 4 ),
 ( 0.01878087663358380885, 0.01956282976579720376, 0.02034478289801060213, 0.02112673603022399704, 0.02190868916243739195, 0.02269064229465078686, 0.02347259542686418177, 0.02425454855907758014, 0.02503650169129097505 ),
 .UNSPECIFIED. ) ;
#11540 = CARTESIAN_POINT ( 'NONE',  ( -1.453535542772826039, -31.06601413805601908, -6.500000000000000000 ) ) ;
#11541 = CARTESIAN_POINT ( 'NONE',  ( 23.03192121915348878, 17.71952646323466496, 11.16877607737301226 ) ) ;
#11542 = DIRECTION ( 'NONE',  ( 0.000000000000000000, 0.000000000000000000, -1.000000000000000000 ) ) ;
#11543 = EDGE_CURVE ( 'NONE', #5355, #1894, #16288, .T. ) ;
#11544 = CARTESIAN_POINT ( 'NONE',  ( 2.000000000000000888, 26.72500000000000142, 12.46410161513774817 ) ) ;
#11545 = CARTESIAN_POINT ( 'NONE',  ( 22.10157009459123856, 19.44537271663178757, 5.746835883940462963 ) ) ;
#11546 = CARTESIAN_POINT ( 'NONE',  ( -2.000000000000000888, -29.36874999877096926, 12.46410161513774817 ) ) ;
#11547 = ORIENTED_EDGE ( 'NONE', *, *, #19209, .T. ) ;
#11548 = B_SPLINE_CURVE_WITH_KNOTS ( 'NONE', 3,
 ( #1902, #14055, #16149, #6194, #21901, #17592, #9987, #23604 ),
 .UNSPECIFIED., .F., .F.,
 ( 4, 2, 2, 4 ),
 ( 0.0009289288217882846459, 0.001160777380751506918, 0.001392625939714729408, 0.001856323057641173302 ),
 .UNSPECIFIED. ) ;
#11549 = ORIENTED_EDGE ( 'NONE', *, *, #21165, .T. ) ;
#11550 = CARTESIAN_POINT ( 'NONE',  ( -1.999999999999998224, 27.04374999877097352, 12.46410161513774639 ) ) ;
#11551 = ORIENTED_EDGE ( 'NONE', *, *, #5464, .T. ) ;
#11552 = CARTESIAN_POINT ( 'NONE',  ( 3.756430356250003655, 28.40312499938548640, 8.999999999999992895 ) ) ;
#11553 = CARTESIAN_POINT ( 'NONE',  ( 15.03485793497900680, 20.69171218447132077, 11.30940107675849404 ) ) ;
#11554 = ORIENTED_EDGE ( 'NONE', *, *, #8385, .F. ) ;
#11555 = EDGE_CURVE ( 'NONE', #10376, #20210, #15514, .T. ) ;
#11556 = ORIENTED_EDGE ( 'NONE', *, *, #16516, .F. ) ;
#11557 = CARTESIAN_POINT ( 'NONE',  ( 2.000000000000005329, 25.07500000000000284, 5.535898384862238508 ) ) ;
#11558 = ORIENTED_EDGE ( 'NONE', *, *, #6198, .F. ) ;
#11559 = ADVANCED_FACE ( 'NONE', ( #6471 ), #1063, .T. ) ;
#11560 = CYLINDRICAL_SURFACE ( 'NONE', #16432, 31.10000000000000142 ) ;
#11561 = CARTESIAN_POINT ( 'NONE',  ( -3.999999999999996447, -8.999999999999992895, 4.218749998770966236 ) ) ;
#11562 = CARTESIAN_POINT ( 'NONE',  ( 0.000000000000000000, 28.62812499938549138, 13.33755215474603162 ) ) ;
#11563 = EDGE_CURVE ( 'NONE', #9293, #20546, #18109, .T. ) ;
#11564 = DIRECTION ( 'NONE',  ( -0.000000000000000000, -0.000000000000000000, 1.000000000000000000 ) ) ;
#11565 = CARTESIAN_POINT ( 'NONE',  ( 2.000000000000003553, 25.97500000000000497, 5.535898384862238508 ) ) ;
#11566 = CARTESIAN_POINT ( 'NONE',  ( 1.878215178125000939, 27.76562499938548356, 12.25316411605952283 ) ) ;
#11567 = CARTESIAN_POINT ( 'NONE',  ( -25.16042852506104666, -18.28012134629567598, 1.000000000000000000 ) ) ;
#11568 = DIRECTION ( 'NONE',  ( 1.000000000000000000, 0.000000000000000000, 0.000000000000000000 ) ) ;
#11569 = LINE ( 'NONE', #10483, #20089 ) ;
#11570 = CARTESIAN_POINT ( 'NONE',  ( -25.99519186311192342, 0.5000000000000000000, 19.50000000000000000 ) ) ;
#11571 = CARTESIAN_POINT ( 'NONE',  ( 21.05410440982949183, 18.22567728508322205, 5.535898384862238508 ) ) ;
#11572 = CARTESIAN_POINT ( 'NONE',  ( 16.65886629145492748, 21.97126104737360919, 11.16877607737301226 ) ) ;
#11573 = DIRECTION ( 'NONE',  ( -0.000000000000000000, 0.000000000000000000, -1.000000000000000000 ) ) ;
#11574 =( BOUNDED_CURVE ( )  B_SPLINE_CURVE ( 2, ( #6881, #10539, #24802, #6611, #14357, #4276, #12251 ),
 .UNSPECIFIED., .F., .T. ) 
 B_SPLINE_CURVE_WITH_KNOTS ( ( 3, 2, 2, 3 ),
 ( 0.7000000000000001776, 0.7166666666666667851, 0.7333333333333333925, 0.7500000000000000000 ),
 .UNSPECIFIED. ) 
 CURVE ( )  GEOMETRIC_REPRESENTATION_ITEM ( )  RATIONAL_B_SPLINE_CURVE ( ( 0.9999999999999982236, 0.8660254037844404840, 1.000000000000000000, 0.8660254037844387076, 1.000000000000000000, 0.8660254037844387076, 1.000000000000000000 ) ) 
 REPRESENTATION_ITEM ( '' )  );
#11575 = CYLINDRICAL_SURFACE ( 'NONE', #21147, 4.000000000000000000 ) ;
#11576 = CARTESIAN_POINT ( 'NONE',  ( 0.000000000000000000, 0.000000000000000000, 17.00000000000000000 ) ) ;
#11577 = CARTESIAN_POINT ( 'NONE',  ( 4.000000000000003553, -8.999999999999992895, 0.000000000000000000 ) ) ;
#11578 = ORIENTED_EDGE ( 'NONE', *, *, #11151, .F. ) ;
#11579 = CARTESIAN_POINT ( 'NONE',  ( 3.752267015613588906E-15, 25.95624999877096784, 4.381197846482986158 ) ) ;
#11580 = CARTESIAN_POINT ( 'NONE',  ( -2.000000000000000888, -27.17500000000000071, 12.46410161513774817 ) ) ;
#11582 = EDGE_LOOP ( 'NONE', ( #15337, #21617, #11370, #2461 ) ) ;
#11581 = CARTESIAN_POINT ( 'NONE',  ( 1.878215178125003382, 25.32812499938548356, 5.746835883940462963 ) ) ;
#11583 = CARTESIAN_POINT ( 'NONE',  ( -3.756430356249996994, 25.47812499938548569, 8.999999999999992895 ) ) ;
#11584 =( BOUNDED_CURVE ( )  B_SPLINE_CURVE ( 2, ( #18041, #24039, #13849, #251, #5865, #25872, #126, #14104, #12133 ),
 .UNSPECIFIED., .F., .F. ) 
 B_SPLINE_CURVE_WITH_KNOTS ( ( 3, 2, 2, 2, 3 ),
 ( 0.2750000000000000222, 0.2833333333333333259, 0.2999999999999999889, 0.3166666666666666519, 0.3250000000000000111 ),
 .UNSPECIFIED. ) 
 CURVE ( )  GEOMETRIC_REPRESENTATION_ITEM ( )  RATIONAL_B_SPLINE_CURVE ( ( 0.9330127018922194093, 0.9330127018922196314, 1.000000000000000000, 0.8660254037844387076, 1.000000000000000000, 0.8660254037844387076, 1.000000000000000000, 0.9330127018922191873, 0.9330127018922194093 ) ) 
 REPRESENTATION_ITEM ( '' )  );
#11585 = DIRECTION ( 'NONE',  ( 1.000000000000000000, 0.000000000000000000, 0.000000000000000000 ) ) ;
#11586 = DIRECTION ( 'NONE',  ( -0.000000000000000000, -0.000000000000000000, -1.000000000000000000 ) ) ;
#11587 = ORIENTED_EDGE ( 'NONE', *, *, #1479, .F. ) ;
#11588 = VERTEX_POINT ( 'NONE', #7319 ) ;
#11589 = EDGE_CURVE ( 'NONE', #13240, #1665, #910, .T. ) ;
#11590 = CYLINDRICAL_SURFACE ( 'NONE', #2647, 4.000000000000000000 ) ;
#11591 = CARTESIAN_POINT ( 'NONE',  ( -1.878215178124996498, 29.00312499938548783, 5.746835883940462963 ) ) ;
#11592 = EDGE_CURVE ( 'NONE', #21926, #20454, #2151, .T. ) ;
#11593 = CARTESIAN_POINT ( 'NONE',  ( 3.756430356250002323, -11.16877607737301403, 1.003124999385480498 ) ) ;
#11594 = EDGE_CURVE ( 'NONE', #14918, #4583, #21688, .T. ) ;
#11595 = AXIS2_PLACEMENT_3D ( 'NONE', #3042, #1076, #1196 ) ;
#11596 = CARTESIAN_POINT ( 'NONE',  ( 0.000000000000000000, 0.000000000000000000, 20.00000000000000000 ) ) ;
#11597 = DIRECTION ( 'NONE',  ( -0.000000000000000000, -0.000000000000000000, -1.000000000000000000 ) ) ;
#11598 = DIRECTION ( 'NONE',  ( 0.000000000000000000, 0.000000000000000000, 1.000000000000000000 ) ) ;
#11599 = CARTESIAN_POINT ( 'NONE',  ( 20.74032577480890183, 20.74032577480883077, 12.99999999999999289 ) ) ;
#11600 = CIRCLE ( 'NONE', #25404, 0.4999999999999999445 ) ;
#11601 = CARTESIAN_POINT ( 'NONE',  ( 29.99470236596032535, 8.217531866531109230, 1.000000000000000000 ) ) ;
#11602 = CARTESIAN_POINT ( 'NONE',  ( -1.453535542772826039, -31.06601413805601908, 1.000000000000000000 ) ) ;
#11603 = LINE ( 'NONE', #13971, #3284 ) ;
#11604 = CARTESIAN_POINT ( 'NONE',  ( -22.67092431280609688, -21.28941499438201745, -6.500000000000000000 ) ) ;
#11605 = EDGE_LOOP ( 'NONE', ( #22535, #22394, #3816, #19591 ) ) ;
#11606 = DIRECTION ( 'NONE',  ( -0.000000000000000000, -1.000000000000000000, -0.000000000000000000 ) ) ;
#11607 = CARTESIAN_POINT ( 'NONE',  ( 4.000000000000003553, 29.73213749463701561, 8.999999999999992895 ) ) ;
#11608 = CARTESIAN_POINT ( 'NONE',  ( 2.672651547586948120E-15, 28.74062499938548498, 13.33755215474602984 ) ) ;
#11609 = CARTESIAN_POINT ( 'NONE',  ( 19.67524618651571799, 16.84681906176946242, 12.46410161513774817 ) ) ;
#11610 = CARTESIAN_POINT ( 'NONE',  ( -1.999999999999998224, -12.46410161513774639, 4.349999999999999645 ) ) ;
#11611 = DIRECTION ( 'NONE',  ( 1.000000000000000000, 0.000000000000000000, 0.000000000000000000 ) ) ;
#11612 = ORIENTED_EDGE ( 'NONE', *, *, #3705, .T. ) ;
#11613 = CARTESIAN_POINT ( 'NONE',  ( 3.137519842735244810E-15, -26.85624999877096641, 4.999999999999991118 ) ) ;
#11614 = CARTESIAN_POINT ( 'NONE',  ( -5.357084559935323398, 38.69843056730299224, 6.772139184627471664 ) ) ;
#11616 = VERTEX_POINT ( 'NONE', #9668 ) ;
#11615 = CARTESIAN_POINT ( 'NONE',  ( -9.610428525060479288, 29.57785765677940404, 1.000000000000000000 ) ) ;
#11617 = ORIENTED_EDGE ( 'NONE', *, *, #24680, .T. ) ;
#11618 = AXIS2_PLACEMENT_3D ( 'NONE', #6926, #20787, #17271 ) ;
#11619 = ORIENTED_EDGE ( 'NONE', *, *, #25079, .F. ) ;
#11620 = ORIENTED_EDGE ( 'NONE', *, *, #20025, .T. ) ;
#11621 = ORIENTED_EDGE ( 'NONE', *, *, #1898, .F. ) ;
#11622 = EDGE_CURVE ( 'NONE', #16822, #19025, #13334, .T. ) ;
#11623 = CYLINDRICAL_SURFACE ( 'NONE', #1364, 31.10000000000000142 ) ;
#11624 = LINE ( 'NONE', #15958, #1509 ) ;
#11626 = EDGE_CURVE ( 'NONE', #20014, #256, #3389, .T. ) ;
#11625 = CIRCLE ( 'NONE', #427, 0.5000000000000002220 ) ;
#11627 = CIRCLE ( 'NONE', #19149, 0.4999999999999986122 ) ;
#11628 = CARTESIAN_POINT ( 'NONE',  ( -25.16042852506064165, 18.28012134629622309, -6.500000000000000000 ) ) ;
#11629 = CARTESIAN_POINT ( 'NONE',  ( -1.071796769724485232, 27.83259618943233704, 4.999999999999992006 ) ) ;
#11630 = CARTESIAN_POINT ( 'NONE',  ( 3.756430356250002323, -11.16877607737301226, 3.253124999385482941 ) ) ;
#11631 = CARTESIAN_POINT ( 'NONE',  ( 4.000000000000003553, -6.690598923241489970, 1.781249998770966680 ) ) ;
#11632 = CARTESIAN_POINT ( 'NONE',  ( -1.878215178124995832, 29.00312499938548427, 5.746835883940462963 ) ) ;
#11633 = ADVANCED_FACE ( 'NONE', ( #7438 ), #17652, .F. ) ;
#11634 = DIRECTION ( 'NONE',  ( 0.000000000000000000, 0.000000000000000000, 1.000000000000000000 ) ) ;
#11635 = VECTOR ( 'NONE', #18795, 1000.000000000000000 ) ;
#11636 = DIRECTION ( 'NONE',  ( 0.000000000000000000, 0.000000000000000000, 1.000000000000000000 ) ) ;
#11637 = CARTESIAN_POINT ( 'NONE',  ( 3.752267015613588906E-15, -4.381197846482986158, 2.812499999999997335 ) ) ;
#11638 = CIRCLE ( 'NONE', #3702, 0.5000000000000003331 ) ;
#11639 = CARTESIAN_POINT ( 'NONE',  ( -14.48253926456298579, 27.25313774936435962, 1.000000000000000000 ) ) ;
#11640 = CARTESIAN_POINT ( 'NONE',  ( 3.999999999999995559, -25.58124999877096784, 6.690598923241487306 ) ) ;
#11641 = CARTESIAN_POINT ( 'NONE',  ( 26.52310962334744104, 16.23990935651718459, 1.000000000000000000 ) ) ;
#11642 = CARTESIAN_POINT ( 'NONE',  ( -2.620986760973688460E-15, -27.53124999877097068, 13.61880215351699874 ) ) ;
#11643 = CARTESIAN_POINT ( 'NONE',  ( -3.756430356249995661, 28.59062499938548640, 6.831223922626973533 ) ) ;
#11644 = DIRECTION ( 'NONE',  ( 1.000000000000000000, 0.000000000000000000, 0.000000000000000000 ) ) ;
#11646 = CARTESIAN_POINT ( 'NONE',  ( -3.999999999999936051, -11.30940107675852779, 4.706249998770969611 ) ) ;
#11645 = AXIS2_PLACEMENT_3D ( 'NONE', #10841, #543, #6805 ) ;
#11647 = DIRECTION ( 'NONE',  ( 1.000000000000000000, 0.000000000000000000, 0.000000000000000000 ) ) ;
#11648 = VERTEX_POINT ( 'NONE', #15426 ) ;
#11649 = DIRECTION ( 'NONE',  ( 1.000000000000000000, 0.000000000000000000, 0.000000000000000000 ) ) ;
#11650 = ORIENTED_EDGE ( 'NONE', *, *, #2012, .F. ) ;
#11651 = ORIENTED_EDGE ( 'NONE', *, *, #19707, .F. ) ;
#11652 = DIRECTION ( 'NONE',  ( 1.000000000000000000, 0.000000000000000000, 0.000000000000000000 ) ) ;
#11653 = ORIENTED_EDGE ( 'NONE', *, *, #22431, .F. ) ;
#11654 = CARTESIAN_POINT ( 'NONE',  ( -3.756430356250003655, -27.50312499938548427, 8.999999999999992895 ) ) ;
#11655 = ORIENTED_EDGE ( 'NONE', *, *, #24388, .F. ) ;
#11656 = DIRECTION ( 'NONE',  ( 1.000000000000000000, 0.000000000000000000, -0.000000000000000000 ) ) ;
#11657 = AXIS2_PLACEMENT_3D ( 'NONE', #20536, #14406, #2628 ) ;
#11658 = EDGE_LOOP ( 'NONE', ( #2849, #8127, #8800, #8993 ) ) ;
#11660 = CARTESIAN_POINT ( 'NONE',  ( 2.000000000000003997, 26.42500000000000071, 5.535898384862238508 ) ) ;
#11659 =( BOUNDED_CURVE ( )  B_SPLINE_CURVE ( 2, ( #4624, #9064, #12607, #22684, #709, #20582, #972, #19123, #8954 ),
 .UNSPECIFIED., .F., .F. ) 
 B_SPLINE_CURVE_WITH_KNOTS ( ( 3, 2, 2, 2, 3 ),
 ( 0.4250000000000000444, 0.4333333333333333481, 0.4500000000000000111, 0.4666666666666666741, 0.4750000000000000333 ),
 .UNSPECIFIED. ) 
 CURVE ( )  GEOMETRIC_REPRESENTATION_ITEM ( )  RATIONAL_B_SPLINE_CURVE ( ( 0.9330127018922194093, 0.9330127018922196314, 1.000000000000000000, 0.8660254037844387076, 1.000000000000000000, 0.8660254037844387076, 1.000000000000000000, 0.9330127018922191873, 0.9330127018922194093 ) ) 
 REPRESENTATION_ITEM ( '' )  );
#11661 = DIRECTION ( 'NONE',  ( 0.000000000000000000, -0.000000000000000000, 1.000000000000000000 ) ) ;
#11662 = AXIS2_PLACEMENT_3D ( 'NONE', #1876, #12315, #20023 ) ;
#11663 = VECTOR ( 'NONE', #19814, 1000.000000000000000 ) ;
#11664 = EDGE_CURVE ( 'NONE', #5385, #24155, #3573, .T. ) ;
#11665 = CARTESIAN_POINT ( 'NONE',  ( 1.878215178125004048, -5.746835883940462963, 0.7781249993854856273 ) ) ;
#11666 = CARTESIAN_POINT ( 'NONE',  ( -4.000000000000000000, 25.67500000000000426, 8.999999999999992895 ) ) ;
#11667 = CARTESIAN_POINT ( 'NONE',  ( 21.99550407741325486, 19.33930669945380743, 12.25316411605952283 ) ) ;
#11668 = DIRECTION ( 'NONE',  ( 0.9822872507286911636, 0.1873813145857119722, 0.000000000000000000 ) ) ;
#11669 = LINE ( 'NONE', #16958, #3768 ) ;
#11670 = AXIS2_PLACEMENT_3D ( 'NONE', #12819, #20791, #22493 ) ;
#11671 = CARTESIAN_POINT ( 'NONE',  ( -1.999999999999998224, 27.10000000000000142, 12.46410161513774639 ) ) ;
#11672 = EDGE_CURVE ( 'NONE', #17557, #8943, #8097, .T. ) ;
#11673 = AXIS2_PLACEMENT_3D ( 'NONE', #13282, #25056, #5432 ) ;
#11674 = CARTESIAN_POINT ( 'NONE',  ( -1.071796769724488563, 29.36740381056767291, 12.99999999999999289 ) ) ;
#11675 = CARTESIAN_POINT ( 'NONE',  ( 17.61346044605677008, 22.92585520197543758, 11.16877607737301048 ) ) ;
#11676 = CARTESIAN_POINT ( 'NONE',  ( 1.487416814333745711E-14, 28.03750000000001208, 12.99999999999999289 ) ) ;
#11677 = ORIENTED_EDGE ( 'NONE', *, *, #8562, .F. ) ;
#11678 = VERTEX_POINT ( 'NONE', #373 ) ;
#11679 = CARTESIAN_POINT ( 'NONE',  ( -3.756430356249996105, 25.44062499938548783, 6.831223922626973533 ) ) ;
#11680 = AXIS2_PLACEMENT_3D ( 'NONE', #21289, #11347, #1421 ) ;
#11681 = ORIENTED_EDGE ( 'NONE', *, *, #5656, .F. ) ;
#11682 = CARTESIAN_POINT ( 'NONE',  ( 2.000000000000000888, 26.27499999999999858, 12.46410161513774817 ) ) ;
#11683 = AXIS2_PLACEMENT_3D ( 'NONE', #15722, #11529, #23569 ) ;
#11684 = CARTESIAN_POINT ( 'NONE',  ( -1.999999999999996669, 29.35000000000000853, 12.46410161513774639 ) ) ;
#11685 = CARTESIAN_POINT ( 'NONE',  ( 4.000000000000001776, 28.05624999877096570, 11.30940107675849760 ) ) ;
#11686 = ORIENTED_EDGE ( 'NONE', *, *, #16598, .T. ) ;
#11687 = EDGE_LOOP ( 'NONE', ( #18675, #23575, #20847 ) ) ;
#11688 = CYLINDRICAL_SURFACE ( 'NONE', #1083, 0.5000000000000004441 ) ;
#11689 = CIRCLE ( 'NONE', #433, 0.5000000000000003331 ) ;
#11690 = ORIENTED_EDGE ( 'NONE', *, *, #5988, .F. ) ;
#11691 = ADVANCED_FACE ( 'NONE', ( #8482 ), #4029, .T. ) ;
#11692 = CARTESIAN_POINT ( 'NONE',  ( 3.077103717553398621, 38.94033362033496815, 4.369373194502302660 ) ) ;
#11693 = DIRECTION ( 'NONE',  ( 0.000000000000000000, 0.000000000000000000, -1.000000000000000000 ) ) ;
#11694 = CARTESIAN_POINT ( 'NONE',  ( -3.756430356249997882, 28.02812499938548996, 6.831223922626973533 ) ) ;
#11695 = CIRCLE ( 'NONE', #2111, 0.5000000000000006661 ) ;
#11696 =( BOUNDED_SURFACE ( )  B_SPLINE_SURFACE ( 1, 2, ( 
 ( #13123, #3051, #965, #6844, #16650, #2784, #5007, #6703, #4877, #7098, #14698, #17178, #6966, #22678, #22799, #9057, #12990, #4763, #12732, #10747, #825, #1084, #20970, #8947, #21093, #15215, #12852, #3171, #20826, #16922, #8803, #15083, #24762, #11138, #19116, #19000, #2914, #10878, #25009, #1205, #18877, #9188, #25146, #9709, #7478, #15468, #23686, #17555, #13376, #23302, #1598, #11795, #5650, #5388, #9828, #21350, #25660, #15847, #21599, #3678, #11654, #25392, #23819, #19631, #13630, #15724, #1736, #23436, #17813, #15333, #7860, #1475, #1867, #5524, #17691, #11408, #15599, #23572, #7741, #13513, #25778, #3434, #5906, #9447, #21213, #21483, #5768, #19381, #13752, #21731, #3556, #3292, #3815, #11531, #19771, #11264, #19251, #19499, #1349, #9326, #17311, #9567, #25275, #7615, #7357, #17427, #25531, #19883, #3949, #761, #10425, #20769, #16339, #520, #18423, #16721, #20641, #22341, #11915, #2459, #14499 ),
 ( #14383, #24308, #6514, #14765, #18676, #644, #24552, #6394, #6639, #22741, #8733, #8490, #4819, #4424, #2847, #24694, #14629, #12529, #16476, #24828, #12399, #16593, #1984, #24438, #6780, #9951, #10814, #10564, #8879, #22467, #2723, #8612, #21866, #16863, #13893, #17938, #12672, #22609, #20505, #12795, #896, #4547, #18808, #2604, #18561, #8003, #28, #20364, #4694, #10687, #13185, #18944, #10956, #5324, #21155, #12922, #9503, #19321, #21279, #19058, #1142, #9388, #3227, #24946, #9002, #11198, #23369, #17249, #16981, #21417, #7026, #11337, #1532, #7297, #15276, #23241, #11079, #17484, #13305, #25217, #1415, #15393, #19179, #1276, #3361, #15014, #17368, #25335, #9115, #25081, #2986, #23125, #6904, #7167, #22994, #1027, #7413, #4938, #5455, #13448, #3498, #11470, #19440, #14887, #22862, #9260, #20898, #5079, #13060, #21038, #3114, #17106, #15157, #5208, #7799, #21535, #13570, #3617, #18010, #12105, #11854 ) ),
 .UNSPECIFIED., .F., .F., .T. ) 
 B_SPLINE_SURFACE_WITH_KNOTS ( ( 2, 2 ),
 ( 3, 2, 2, 2, 2, 2, 2, 2, 2, 2, 2, 2, 2, 2, 2, 2, 2, 2, 2, 2, 2, 2, 2, 2, 2, 2, 2, 2, 2, 2, 2, 2, 2, 2, 2, 2, 2, 2, 2, 2, 2, 2, 2, 2, 2, 2, 2, 2, 2, 2, 2, 2, 2, 2, 2, 2, 2, 2, 2, 2, 3 ),
 ( 0.000000000000000000, 1.000000000000000000 ),
 ( 0.000000000000000000, 0.01666666666666666644, 0.03333333333333333287, 0.05000000000000000278, 0.06666666666666666574, 0.08333333333333332871, 0.1000000000000000056, 0.1166666666666666685, 0.1333333333333333315, 0.1499999999999999944, 0.1666666666666666574, 0.1833333333333333204, 0.2000000000000000111, 0.2166666666666666741, 0.2333333333333333370, 0.2500000000000000000, 0.2666666666666666630, 0.2833333333333333259, 0.2999999999999999889, 0.3166666666666666519, 0.3333333333333333148, 0.3499999999999999778, 0.3666666666666666408, 0.3833333333333333592, 0.4000000000000000222, 0.4166666666666666852, 0.4333333333333333481, 0.4500000000000000111, 0.4666666666666666741, 0.4833333333333333370, 0.5000000000000000000, 0.5166666666666667185, 0.5333333333333333259, 0.5500000000000000444, 0.5666666666666666519, 0.5833333333333333703, 0.5999999999999999778, 0.6166666666666666963, 0.6333333333333333037, 0.6500000000000000222, 0.6666666666666666297, 0.6833333333333333481, 0.6999999999999999556, 0.7166666666666666741, 0.7333333333333332815, 0.7500000000000000000, 0.7666666666666667185, 0.7833333333333333259, 0.8000000000000000444, 0.8166666666666666519, 0.8333333333333333703, 0.8499999999999999778, 0.8666666666666666963, 0.8833333333333333037, 0.9000000000000000222, 0.9166666666666666297, 0.9333333333333333481, 0.9499999999999999556, 0.9666666666666666741, 0.9833333333333332815, 1.000000000000000000 ),
 .UNSPECIFIED. ) 
 GEOMETRIC_REPRESENTATION_ITEM ( )  RATIONAL_B_SPLINE_SURFACE ( (
 ( 1.000000000000000000, 0.8660254037844387076, 1.000000000000000000, 0.8660254037844387076, 1.000000000000000000, 0.8660254037844387076, 1.000000000000000000, 0.8660254037844387076, 1.000000000000000000, 0.8660254037844387076, 1.000000000000000000, 0.8660254037844387076, 1.000000000000000000, 0.8660254037844387076, 1.000000000000000000, 0.8660254037844387076, 1.000000000000000000, 0.8660254037844387076, 1.000000000000000000, 0.8660254037844387076, 1.000000000000000000, 0.8660254037844387076, 1.000000000000000000, 0.8660254037844387076, 1.000000000000000000, 0.8660254037844387076, 1.000000000000000000, 0.8660254037844387076, 1.000000000000000000, 0.8660254037844387076, 1.000000000000000000, 0.8660254037844387076, 1.000000000000000000, 0.8660254037844387076, 1.000000000000000000, 0.8660254037844387076, 1.000000000000000000, 0.8660254037844387076, 1.000000000000000000, 0.8660254037844387076, 1.000000000000000000, 0.8660254037844387076, 1.000000000000000000, 0.8660254037844387076, 1.000000000000000000, 0.8660254037844387076, 1.000000000000000000, 0.8660254037844387076, 1.000000000000000000, 0.8660254037844387076, 1.000000000000000000, 0.8660254037844387076, 1.000000000000000000, 0.8660254037844387076, 1.000000000000000000, 0.8660254037844387076, 1.000000000000000000, 0.8660254037844387076, 1.000000000000000000, 0.8660254037844387076, 1.000000000000000000, 0.8660254037844387076, 1.000000000000000000, 0.8660254037844387076, 1.000000000000000000, 0.8660254037844387076, 1.000000000000000000, 0.8660254037844387076, 1.000000000000000000, 0.8660254037844387076, 1.000000000000000000, 0.8660254037844387076, 1.000000000000000000, 0.8660254037844387076, 1.000000000000000000, 0.8660254037844387076, 1.000000000000000000, 0.8660254037844387076, 1.000000000000000000, 0.8660254037844387076, 1.000000000000000000, 0.8660254037844387076, 1.000000000000000000, 0.8660254037844387076, 1.000000000000000000, 0.8660254037844387076, 1.000000000000000000, 0.8660254037844387076, 1.000000000000000000, 0.8660254037844387076, 1.000000000000000000, 0.8660254037844387076, 1.000000000000000000, 0.8660254037844387076, 1.000000000000000000, 0.8660254037844387076, 1.000000000000000000, 0.8660254037844387076, 1.000000000000000000, 0.8660254037844387076, 1.000000000000000000, 0.8660254037844387076, 1.000000000000000000, 0.8660254037844387076, 1.000000000000000000, 0.8660254037844387076, 1.000000000000000000, 0.8660254037844387076, 1.000000000000000000, 0.8660254037844387076, 1.000000000000000000, 0.8660254037844387076, 1.000000000000000000, 0.8660254037844387076, 1.000000000000000000, 0.8660254037844387076, 1.000000000000000000, 0.8660254037844387076, 1.000000000000000000, 0.8660254037844387076, 1.000000000000000000),
 ( 1.000000000000000000, 0.8660254037844387076, 1.000000000000000000, 0.8660254037844387076, 1.000000000000000000, 0.8660254037844387076, 1.000000000000000000, 0.8660254037844387076, 1.000000000000000000, 0.8660254037844387076, 1.000000000000000000, 0.8660254037844387076, 1.000000000000000000, 0.8660254037844387076, 1.000000000000000000, 0.8660254037844387076, 1.000000000000000000, 0.8660254037844387076, 1.000000000000000000, 0.8660254037844387076, 1.000000000000000000, 0.8660254037844387076, 1.000000000000000000, 0.8660254037844387076, 1.000000000000000000, 0.8660254037844387076, 1.000000000000000000, 0.8660254037844387076, 1.000000000000000000, 0.8660254037844387076, 1.000000000000000000, 0.8660254037844387076, 1.000000000000000000, 0.8660254037844387076, 1.000000000000000000, 0.8660254037844387076, 1.000000000000000000, 0.8660254037844387076, 1.000000000000000000, 0.8660254037844387076, 1.000000000000000000, 0.8660254037844387076, 1.000000000000000000, 0.8660254037844387076, 1.000000000000000000, 0.8660254037844387076, 1.000000000000000000, 0.8660254037844387076, 1.000000000000000000, 0.8660254037844387076, 1.000000000000000000, 0.8660254037844387076, 1.000000000000000000, 0.8660254037844387076, 1.000000000000000000, 0.8660254037844387076, 1.000000000000000000, 0.8660254037844387076, 1.000000000000000000, 0.8660254037844387076, 1.000000000000000000, 0.8660254037844387076, 1.000000000000000000, 0.8660254037844387076, 1.000000000000000000, 0.8660254037844387076, 1.000000000000000000, 0.8660254037844387076, 1.000000000000000000, 0.8660254037844387076, 1.000000000000000000, 0.8660254037844387076, 1.000000000000000000, 0.8660254037844387076, 1.000000000000000000, 0.8660254037844387076, 1.000000000000000000, 0.8660254037844387076, 1.000000000000000000, 0.8660254037844387076, 1.000000000000000000, 0.8660254037844387076, 1.000000000000000000, 0.8660254037844387076, 1.000000000000000000, 0.8660254037844387076, 1.000000000000000000, 0.8660254037844387076, 1.000000000000000000, 0.8660254037844387076, 1.000000000000000000, 0.8660254037844387076, 1.000000000000000000, 0.8660254037844387076, 1.000000000000000000, 0.8660254037844387076, 1.000000000000000000, 0.8660254037844387076, 1.000000000000000000, 0.8660254037844387076, 1.000000000000000000, 0.8660254037844387076, 1.000000000000000000, 0.8660254037844387076, 1.000000000000000000, 0.8660254037844387076, 1.000000000000000000, 0.8660254037844387076, 1.000000000000000000, 0.8660254037844387076, 1.000000000000000000, 0.8660254037844387076, 1.000000000000000000, 0.8660254037844387076, 1.000000000000000000, 0.8660254037844387076, 1.000000000000000000, 0.8660254037844387076, 1.000000000000000000, 0.8660254037844387076, 1.000000000000000000) ) ) 
 REPRESENTATION_ITEM ( '' )  SURFACE ( )  );
#11697 = CARTESIAN_POINT ( 'NONE',  ( 0.000000000000000000, 0.000000000000000000, -6.500000000000000000 ) ) ;
#11698 = CARTESIAN_POINT ( 'NONE',  ( -3.999999999999998224, 26.12500000000001066, 8.999999999999992895 ) ) ;
#11699 = EDGE_CURVE ( 'NONE', #14590, #23126, #8942, .T. ) ;
#11700 = DIRECTION ( 'NONE',  ( -0.000000000000000000, 1.000000000000000000, 0.000000000000000000 ) ) ;
#11701 = ADVANCED_FACE ( 'NONE', ( #2453 ), #20358, .F. ) ;
#11702 = CARTESIAN_POINT ( 'NONE',  ( 4.000000000000003553, -8.999999999999992895, 0.000000000000000000 ) ) ;
#11703 = DIRECTION ( 'NONE',  ( 0.000000000000000000, 0.000000000000000000, 1.000000000000000000 ) ) ;
#11704 = VECTOR ( 'NONE', #24131, 1000.000000000000000 ) ;
#11705 = FACE_OUTER_BOUND ( 'NONE', #3613, .T. ) ;
#11706 = CARTESIAN_POINT ( 'NONE',  ( 18.55271417138207468, 18.55271417138200718, 13.61880215351699874 ) ) ;
#11707 = CARTESIAN_POINT ( 'NONE',  ( 23.35011927068743276, 18.03772451476861605, 11.16877607737301226 ) ) ;
#11708 = EDGE_CURVE ( 'NONE', #8133, #17209, #11584, .T. ) ;
#11709 = CARTESIAN_POINT ( 'NONE',  ( -3.999999999999996447, -8.999999999999992895, 4.668749998770968190 ) ) ;
#11710 = LINE ( 'NONE', #25706, #12248 ) ;
#11711 = AXIS2_PLACEMENT_3D ( 'NONE', #3631, #17380, #19335 ) ;
#11712 = CARTESIAN_POINT ( 'NONE',  ( 4.000000000000002665, 27.23124999877097352, 6.690598923241489970 ) ) ;
#11713 = VECTOR ( 'NONE', #14779, 1000.000000000000000 ) ;
#11714 = CARTESIAN_POINT ( 'NONE',  ( 19.52492222951535439, 22.18111960747465261, 12.25316411605951927 ) ) ;
#11715 = CARTESIAN_POINT ( 'NONE',  ( 3.959305671612554781E-15, 25.00000000000000000, 12.99999999999999289 ) ) ;
#11716 = ORIENTED_EDGE ( 'NONE', *, *, #22294, .F. ) ;
#11717 = CARTESIAN_POINT ( 'NONE',  ( 2.000000000000003997, 26.36874999877096926, 5.535898384862238508 ) ) ;
#11718 = CARTESIAN_POINT ( 'NONE',  ( -2.000000000000000888, -26.72500000000000142, 12.46410161513774817 ) ) ;
#11720 = ORIENTED_EDGE ( 'NONE', *, *, #3022, .T. ) ;
#11719 = CARTESIAN_POINT ( 'NONE',  ( 1.878215178124999829, 25.62812499938549138, 12.25316411605952283 ) ) ;
#11721 = CARTESIAN_POINT ( 'NONE',  ( 3.756430356250003655, 29.30312499938548498, 8.999999999999992895 ) ) ;
#11722 = VECTOR ( 'NONE', #24448, 1000.000000000000000 ) ;
#11723 = CARTESIAN_POINT ( 'NONE',  ( 0.000000000000000000, 0.000000000000000000, 17.69999999999999929 ) ) ;
#11724 = CARTESIAN_POINT ( 'NONE',  ( 6.741346781237198549, 25.16843286583315020, 20.00001200000000168 ) ) ;
#11725 = LINE ( 'NONE', #19824, #9215 ) ;
#11726 = VERTEX_POINT ( 'NONE', #5999 ) ;
#11727 = ORIENTED_EDGE ( 'NONE', *, *, #18420, .F. ) ;
#11728 =( LENGTH_UNIT ( ) NAMED_UNIT ( * ) SI_UNIT ( .MILLI., .METRE. ) );
#11729 = CARTESIAN_POINT ( 'NONE',  ( -1.878215178124999829, 29.15312499938549351, 12.25316411605951927 ) ) ;
#11730 = CARTESIAN_POINT ( 'NONE',  ( -1.878215178124995832, -5.746835883940462963, 3.440624999385483829 ) ) ;
#11731 = CIRCLE ( 'NONE', #10069, 0.5000000000000004441 ) ;
#11732 = AXIS2_PLACEMENT_3D ( 'NONE', #19834, #15791, #24144 ) ;
#11733 = DIRECTION ( 'NONE',  ( -0.000000000000000000, 1.000000000000000000, 0.000000000000000000 ) ) ;
#11734 = DIRECTION ( 'NONE',  ( -0.000000000000000000, -0.000000000000000000, -1.000000000000000000 ) ) ;
#11735 = VECTOR ( 'NONE', #19924, 1000.000000000000000 ) ;
#11736 = CARTESIAN_POINT ( 'NONE',  ( 19.19352969096333439, 22.02195681570944785, 5.535898384862237620 ) ) ;
#11737 = FACE_OUTER_BOUND ( 'NONE', #16620, .T. ) ;
#11738 = CARTESIAN_POINT ( 'NONE',  ( -1.071796769724488563, 26.66740381056766651, 12.99999999999999289 ) ) ;
#11739 = DIRECTION ( 'NONE',  ( 0.000000000000000000, 0.000000000000000000, 1.000000000000000000 ) ) ;
#11740 = CARTESIAN_POINT ( 'NONE',  ( 7.437084071668728555E-15, 26.63124999877097565, 12.99999999999999112 ) ) ;
#11741 = ADVANCED_FACE ( 'NONE', ( #22068 ), #20110, .T. ) ;
#11742 = VERTEX_POINT ( 'NONE', #24160 ) ;
#11743 = FACE_BOUND ( 'NONE', #7349, .T. ) ;
#11744 = CARTESIAN_POINT ( 'NONE',  ( 3.756430356249997882, -29.56562499938549138, 11.16877607737301226 ) ) ;
#11745 =( BOUNDED_CURVE ( )  B_SPLINE_CURVE ( 2, ( #20563, #2773, #14682, #10482, #6832, #8541, #12194, #2652, #22523 ),
 .UNSPECIFIED., .F., .F. ) 
 B_SPLINE_CURVE_WITH_KNOTS ( ( 3, 2, 2, 2, 3 ),
 ( 0.7249999999999999778, 0.7333333333333332815, 0.7500000000000000000, 0.7666666666666667185, 0.7750000000000000222 ),
 .UNSPECIFIED. ) 
 CURVE ( )  GEOMETRIC_REPRESENTATION_ITEM ( )  RATIONAL_B_SPLINE_CURVE ( ( 0.9330127018922194093, 0.9330127018922194093, 1.000000000000000000, 0.8660254037844387076, 1.000000000000000000, 0.8660254037844387076, 1.000000000000000000, 0.9330127018922194093, 0.9330127018922194093 ) ) 
 REPRESENTATION_ITEM ( '' )  );
#11746 = CARTESIAN_POINT ( 'NONE',  ( 2.672651547586948120E-15, 26.94062499938548783, 13.33755215474602984 ) ) ;
#11747 = ADVANCED_FACE ( 'NONE', ( #10171 ), #4298, .T. ) ;
#11748 = CARTESIAN_POINT ( 'NONE',  ( -1.499999999999998224, -7.499999999999992895, 4.999999999999993783 ) ) ;
#11749 = VECTOR ( 'NONE', #24771, 1000.000000000000000 ) ;
#11750 = CARTESIAN_POINT ( 'NONE',  ( 5.112995299272250684E-15, 26.01250000000000284, 4.999999999999992006 ) ) ;
#11751 = CARTESIAN_POINT ( 'NONE',  ( 3.756430356250003655, 29.75312499938548783, 8.999999999999992895 ) ) ;
#11752 = VERTEX_POINT ( 'NONE', #12269 ) ;
#11753 = CARTESIAN_POINT ( 'NONE',  ( -3.756430356249996549, 29.52812499938548996, 8.999999999999992895 ) ) ;
#11754 = DIRECTION ( 'NONE',  ( 1.000000000000000000, 0.000000000000000000, 0.000000000000000000 ) ) ;
#11756 = ORIENTED_EDGE ( 'NONE', *, *, #8063, .F. ) ;
#11755 = CARTESIAN_POINT ( 'NONE',  ( 1.071796769724485454, -26.61115380933863150, 12.99999999999999467 ) ) ;
#11757 = ADVANCED_FACE ( 'NONE', ( #23916 ), #2333, .F. ) ;
#11758 = CIRCLE ( 'NONE', #16796, 0.5000000000000001110 ) ;
#11759 = EDGE_LOOP ( 'NONE', ( #2250, #9209, #5520, #20011 ) ) ;
#11760 = ORIENTED_EDGE ( 'NONE', *, *, #20211, .F. ) ;
#11761 = ORIENTED_EDGE ( 'NONE', *, *, #11272, .T. ) ;
#11762 = ORIENTED_EDGE ( 'NONE', *, *, #21233, .T. ) ;
#11763 = DIRECTION ( 'NONE',  ( 0.000000000000000000, 0.000000000000000000, 1.000000000000000000 ) ) ;
#11764 = CYLINDRICAL_SURFACE ( 'NONE', #8033, 4.000000000000000000 ) ;
#11765 = PRESENTATION_STYLE_ASSIGNMENT (( #9805 ) ) ;
#11766 = CARTESIAN_POINT ( 'NONE',  ( -1.071796769724483234, 28.01740381056767148, 12.99999999999999645 ) ) ;
#11767 = CIRCLE ( 'NONE', #9273, 0.5000000000000001110 ) ;
#11768 = CARTESIAN_POINT ( 'NONE',  ( -1.878215178124998497, -12.25316411605951927, 2.690624999385483385 ) ) ;
#11769 = CARTESIAN_POINT ( 'NONE',  ( 4.000000000000003553, -8.999999999999992895, 3.993749998770966592 ) ) ;
#11770 = CIRCLE ( 'NONE', #516, 0.4999999999999995004 ) ;
#11771 = CARTESIAN_POINT ( 'NONE',  ( 1.878215178125004048, 28.02812499938548640, 5.746835883940462963 ) ) ;
#11772 = VECTOR ( 'NONE', #11140, 1000.000000000000000 ) ;
#11773 = FACE_OUTER_BOUND ( 'NONE', #12490, .T. ) ;
#11774 = CARTESIAN_POINT ( 'NONE',  ( 0.000000000000000000, 0.000000000000000000, -6.500000000000000000 ) ) ;
#11775 = EDGE_CURVE ( 'NONE', #13481, #15567, #12601, .T. ) ;
#11776 = CARTESIAN_POINT ( 'NONE',  ( -1.999999999999998224, -12.46410161513774639, 2.550000000000000266 ) ) ;
#11777 = AXIS2_PLACEMENT_3D ( 'NONE', #5806, #9360, #9742 ) ;
#11778 = DIRECTION ( 'NONE',  ( -0.000000000000000000, -0.000000000000000000, -1.000000000000000000 ) ) ;
#11779 = DIRECTION ( 'NONE',  ( 0.000000000000000000, -1.000000000000000000, 0.000000000000000000 ) ) ;
#11780 = DIRECTION ( 'NONE',  ( 1.000000000000000000, 0.000000000000000000, 0.000000000000000000 ) ) ;
#11781 = CARTESIAN_POINT ( 'NONE',  ( -4.000000000000003553, -27.68124999877096926, 6.690598923241489970 ) ) ;
#11782 = VECTOR ( 'NONE', #22315, 1000.000000000000000 ) ;
#11783 = CARTESIAN_POINT ( 'NONE',  ( 2.672651547586948120E-15, 27.84062499938548640, 13.33755215474602984 ) ) ;
#11784 = ADVANCED_FACE ( 'NONE', ( #24300 ), #6386, .F. ) ;
#11785 = CARTESIAN_POINT ( 'NONE',  ( -28.72825533807115050, 11.91206721063083229, -6.500000000000000000 ) ) ;
#11786 = CARTESIAN_POINT ( 'NONE',  ( 6.938893903907228378E-15, 29.50000000000000000, 2.999999999999992450 ) ) ;
#11787 = CYLINDRICAL_SURFACE ( 'NONE', #18509, 2.899999999999999911 ) ;
#11788 = VERTEX_POINT ( 'NONE', #12391 ) ;
#11789 = CARTESIAN_POINT ( 'NONE',  ( 0.000000000000000000, 0.000000000000000000, 1.000000000000000000 ) ) ;
#11790 = VERTEX_POINT ( 'NONE', #11880 ) ;
#11791 = VECTOR ( 'NONE', #15053, 1000.000000000000000 ) ;
#11792 = ORIENTED_EDGE ( 'NONE', *, *, #23192, .F. ) ;
#11793 = DIRECTION ( 'NONE',  ( 0.000000000000000000, 0.000000000000000000, -1.000000000000000000 ) ) ;
#11794 = ORIENTED_EDGE ( 'NONE', *, *, #7727, .F. ) ;
#11795 = CARTESIAN_POINT ( 'NONE',  ( -3.735045420075836212E-15, -27.16562499938548569, 4.662447845253954171 ) ) ;
#11796 = ORIENTED_EDGE ( 'NONE', *, *, #11977, .F. ) ;
#11797 = CARTESIAN_POINT ( 'NONE',  ( -3.999999999999996447, -8.999999999999992895, 2.868749998770965703 ) ) ;
#11798 = VECTOR ( 'NONE', #8629, 1000.000000000000000 ) ;
#11799 = EDGE_CURVE ( 'NONE', #1796, #16142, #19848, .T. ) ;
#11800 = ORIENTED_EDGE ( 'NONE', *, *, #22350, .F. ) ;
#11801 = CARTESIAN_POINT ( 'NONE',  ( -3.999999999999996447, 26.12500000000000355, 8.999999999999992895 ) ) ;
#11802 = CARTESIAN_POINT ( 'NONE',  ( 30.78811501957144969, 4.393401135981008565, 1.000000000000000000 ) ) ;
#11803 = DIRECTION ( 'NONE',  ( 1.000000000000000000, 0.000000000000000000, 0.000000000000000000 ) ) ;
#11804 = DIRECTION ( 'NONE',  ( -0.9048270524660170233, 0.4257792915650782661, 0.000000000000000000 ) ) ;
#11805 = CARTESIAN_POINT ( 'NONE',  ( 15.25349156384666216, 20.56588631976534387, 6.831223922626973533 ) ) ;
#11806 = DIRECTION ( 'NONE',  ( -0.000000000000000000, -0.000000000000000000, -1.000000000000000000 ) ) ;
#11807 = AXIS2_PLACEMENT_3D ( 'NONE', #22344, #6783, #8355 ) ;
#11808 = CARTESIAN_POINT ( 'NONE',  ( 27.09999999999999787, -0.5999999999999998668, 19.59999999999999787 ) ) ;
#11809 = APPLICATION_PROTOCOL_DEFINITION ( 'draft international standard', 'automotive_design', 1998, #12277 ) ;
#11810 = CARTESIAN_POINT ( 'NONE',  ( 4.000000000000003553, 29.08750000000000213, 6.690598923241489970 ) ) ;
#11811 = CARTESIAN_POINT ( 'NONE',  ( 1.878215178125000939, -12.25316411605952283, 0.6281249993854848279 ) ) ;
#11812 = AXIS2_PLACEMENT_3D ( 'NONE', #25267, #7348, #19373 ) ;
#11813 = CARTESIAN_POINT ( 'NONE',  ( 23.35011927068743276, 18.03772451476861605, 11.16877607737301403 ) ) ;
#11814 = CARTESIAN_POINT ( 'NONE',  ( -3.918623196469519065, 34.50000000000000000, 4.456389954662585140 ) ) ;
#11815 = ORIENTED_EDGE ( 'NONE', *, *, #22938, .F. ) ;
#11816 = ORIENTED_EDGE ( 'NONE', *, *, #22866, .F. ) ;
#11817 = CARTESIAN_POINT ( 'NONE',  ( -4.000000000000000888, 29.25624999877096855, 11.30940107675849404 ) ) ;
#11818 = EDGE_CURVE ( 'NONE', #19820, #10854, #14288, .T. ) ;
#11819 = ORIENTED_EDGE ( 'NONE', *, *, #4563, .F. ) ;
#11820 = CARTESIAN_POINT ( 'NONE',  ( -3.999999999999997335, 26.10624999877096997, 11.30940107675849404 ) ) ;
#11821 = CIRCLE ( 'NONE', #3888, 0.4999999999999997224 ) ;
#11822 = DIRECTION ( 'NONE',  ( -0.7071067811865487940, -0.7071067811865463515, 0.000000000000000000 ) ) ;
#11823 = CARTESIAN_POINT ( 'NONE',  ( 14.98182492639001673, 20.63867917588233070, 6.690598923241487306 ) ) ;
#11824 = ORIENTED_EDGE ( 'NONE', *, *, #1130, .T. ) ;
#11825 = VERTEX_POINT ( 'NONE', #2716 ) ;
#11826 = CIRCLE ( 'NONE', #5557, 0.5000000000000005551 ) ;
#11827 = CARTESIAN_POINT ( 'NONE',  ( -1.999999999999995781, -5.535898384862237620, 4.199999999999999289 ) ) ;
#11828 = ORIENTED_EDGE ( 'NONE', *, *, #21358, .F. ) ;
#11829 = CARTESIAN_POINT ( 'NONE',  ( 30.91344420362545975, -3.401318489841207882, -6.500000000000000000 ) ) ;
#11830 = CARTESIAN_POINT ( 'NONE',  ( -22.17092431280609333, -21.28941499438201745, -6.500000000000000000 ) ) ;
#11831 = CARTESIAN_POINT ( 'NONE',  ( 1.878215178125001605, 29.11562499938549209, 12.25316411605952283 ) ) ;
#11832 = CYLINDRICAL_SURFACE ( 'NONE', #2568, 0.5000000000000004441 ) ;
#11833 = CARTESIAN_POINT ( 'NONE',  ( -4.000000000000000000, 27.47500000000000142, 8.999999999999992895 ) ) ;
#11834 = CARTESIAN_POINT ( 'NONE',  ( -3.756430356249995661, 26.22812499938548214, 6.831223922626973533 ) ) ;
#11835 = CARTESIAN_POINT ( 'NONE',  ( 0.000000000000000000, 0.000000000000000000, -6.500000000000000000 ) ) ;
#11836 = PRESENTATION_LAYER_ASSIGNMENT (  '', '', ( #3072 ) ) ;
#11837 = DIRECTION ( 'NONE',  ( -0.000000000000000000, -0.000000000000000000, 1.000000000000000000 ) ) ;
#11838 = CARTESIAN_POINT ( 'NONE',  ( 22.73348301514753800, 17.07662876565508370, 8.999999999999992895 ) ) ;
#11839 = CARTESIAN_POINT ( 'NONE',  ( 22.74023967191403628, 17.42784491599521601, 8.999999999999992895 ) ) ;
#11840 = CARTESIAN_POINT ( 'NONE',  ( -4.000000000000003553, -28.58124999877096784, 6.690598923241489970 ) ) ;
#11841 = DIRECTION ( 'NONE',  ( 0.000000000000000000, 0.000000000000000000, -1.000000000000000000 ) ) ;
#11842 = CARTESIAN_POINT ( 'NONE',  ( -4.000000000000043521, -11.30940107675846562, 2.906249998770967125 ) ) ;
#11843 = ADVANCED_FACE ( 'NONE', ( #12663 ), #636, .T. ) ;
#11844 = CARTESIAN_POINT ( 'NONE',  ( 20.72043839702256207, 20.72043839702248036, 4.662447845253954171 ) ) ;
#11845 = ORIENTED_EDGE ( 'NONE', *, *, #1835, .T. ) ;
#11846 = CARTESIAN_POINT ( 'NONE',  ( 2.000000000000003997, 27.71874999877097068, 5.535898384862238508 ) ) ;
#11847 = CARTESIAN_POINT ( 'NONE',  ( 1.999999999999995781, -26.05000000000000071, 5.535898384862237620 ) ) ;
#11849 = ORIENTED_EDGE ( 'NONE', *, *, #23095, .T. ) ;
#11848 = CARTESIAN_POINT ( 'NONE',  ( 20.64868662990473069, 15.16406212719910052, 8.999999999999992895 ) ) ;
#11850 = CARTESIAN_POINT ( 'NONE',  ( -3.756430356249997438, 29.56562499938549493, 11.16877607737301048 ) ) ;
#11851 = EDGE_CURVE ( 'NONE', #22574, #2153, #7578, .T. ) ;
#11852 = DIRECTION ( 'NONE',  ( 1.000000000000000000, 0.000000000000000000, 0.000000000000000000 ) ) ;
#11853 = ORIENTED_EDGE ( 'NONE', *, *, #5596, .T. ) ;
#11854 = CARTESIAN_POINT ( 'NONE',  ( -3.756430356250003655, -29.64062499938548356, 8.999999999999992895 ) ) ;
#11855 = VERTEX_POINT ( 'NONE', #2594 ) ;
#11856 = ORIENTED_EDGE ( 'NONE', *, *, #11210, .F. ) ;
#11857 = EDGE_CURVE ( 'NONE', #8259, #2175, #22734, .T. ) ;
#11858 = CARTESIAN_POINT ( 'NONE',  ( 5.532151103383234236, 38.49999999999999289, 6.677220593914319657 ) ) ;
#11859 = CARTESIAN_POINT ( 'NONE',  ( -1.878215178124998275, 29.60312499938548925, 12.25316411605951927 ) ) ;
#11860 = CARTESIAN_POINT ( 'NONE',  ( 3.735045420075836212E-15, -4.662447845253954171, 2.953124999385479121 ) ) ;
#11861 = ADVANCED_FACE ( 'NONE', ( #20496 ), #24429, .T. ) ;
#11862 = DIRECTION ( 'NONE',  ( 0.000000000000000000, 0.000000000000000000, -1.000000000000000000 ) ) ;
#11863 =( NAMED_UNIT ( * ) SI_UNIT ( $, .STERADIAN. ) SOLID_ANGLE_UNIT ( ) );
#11864 = DIRECTION ( 'NONE',  ( 0.000000000000000000, 0.000000000000000000, -1.000000000000000000 ) ) ;
#11865 = CARTESIAN_POINT ( 'NONE',  ( -3.959305671612554781E-15, -25.00000000000000000, 12.99999999999999289 ) ) ;
#11866 = DIRECTION ( 'NONE',  ( 1.000000000000000000, 0.000000000000000000, 0.000000000000000000 ) ) ;
#11867 = AXIS2_PLACEMENT_3D ( 'NONE', #20618, #22841, #2822 ) ;
#11868 = CARTESIAN_POINT ( 'NONE',  ( 18.81908170618357090, 17.30333217833144843, 4.999999999999993783 ) ) ;
#11869 = FACE_OUTER_BOUND ( 'NONE', #4421, .T. ) ;
#11870 = CARTESIAN_POINT ( 'NONE',  ( 15.57168961538060969, 20.88408437129928785, 6.831223922626973533 ) ) ;
#11871 = CARTESIAN_POINT ( 'NONE',  ( 16.75401129586974491, 19.58243842061586548, 12.46410161513774639 ) ) ;
#11872 = ORIENTED_EDGE ( 'NONE', *, *, #23066, .T. ) ;
#11873 = CARTESIAN_POINT ( 'NONE',  ( 3.469446951953614189E-15, 25.00000000000000000, 8.999999999999992895 ) ) ;
#11874 = CARTESIAN_POINT ( 'NONE',  ( 5.265192354984335132, 38.83322177420914301, 6.904532280874554395 ) ) ;
#11875 = CARTESIAN_POINT ( 'NONE',  ( 3.756430356250004099, 27.09062499938548285, 6.831223922626973533 ) ) ;
#11876 = CARTESIAN_POINT ( 'NONE',  ( 0.000000000000000000, 0.000000000000000000, 17.69999999999999929 ) ) ;
#11877 = CARTESIAN_POINT ( 'NONE',  ( 3.469446951953614189E-15, 25.00000000000000000, 4.999999999999992006 ) ) ;
#11878 = CARTESIAN_POINT ( 'NONE',  ( 1.453535542772610212, 31.06601413805602263, -6.500000000000000000 ) ) ;
#11879 = ORIENTED_EDGE ( 'NONE', *, *, #8610, .T. ) ;
#11880 = CARTESIAN_POINT ( 'NONE',  ( 1.500000000000001776, -7.499999999999993783, 25.00000000000000000 ) ) ;
#11881 = CARTESIAN_POINT ( 'NONE',  ( 0.7500000000000000000, -2.999999999999999556, 18.19999999999999929 ) ) ;
#11883 = ORIENTED_EDGE ( 'NONE', *, *, #4219, .F. ) ;
#11882 = DIRECTION ( 'NONE',  ( 0.000000000000000000, 0.000000000000000000, 1.000000000000000000 ) ) ;
#11884 = EDGE_LOOP ( 'NONE', ( #16111, #9345, #8065, #21506 ) ) ;
#11885 = VERTEX_POINT ( 'NONE', #20634 ) ;
#11886 = ORIENTED_EDGE ( 'NONE', *, *, #25449, .F. ) ;
#11887 = ADVANCED_FACE ( 'NONE', ( #4930 ), #12913, .T. ) ;
#11888 = DIRECTION ( 'NONE',  ( 0.000000000000000000, 0.000000000000000000, 1.000000000000000000 ) ) ;
#11889 = DIRECTION ( 'NONE',  ( -0.4257792915650782661, -0.9048270524660170233, 0.000000000000000000 ) ) ;
#11890 = EDGE_CURVE ( 'NONE', #10602, #789, #22191, .T. ) ;
#11891 = CARTESIAN_POINT ( 'NONE',  ( -3.756430356249998326, 28.10312499938548569, 11.16877607737301226 ) ) ;
#11892 = EDGE_CURVE ( 'NONE', #24369, #2048, #901, .T. ) ;
#11893 = CARTESIAN_POINT ( 'NONE',  ( 3.756430356250002323, -11.16877607737301226, 2.803124999385479210 ) ) ;
#11894 = CARTESIAN_POINT ( 'NONE',  ( 4.000000000000001776, -11.30940107675849760, 3.956249998770966947 ) ) ;
#11895 =( BOUNDED_CURVE ( )  B_SPLINE_CURVE ( 2, ( #19624, #24069, #17686, #10076, #16105, #25654, #18077, #5899, #9944 ),
 .UNSPECIFIED., .F., .F. ) 
 B_SPLINE_CURVE_WITH_KNOTS ( ( 3, 2, 2, 2, 3 ),
 ( 0.4250000000000000444, 0.4333333333333333481, 0.4500000000000000111, 0.4666666666666666741, 0.4750000000000000333 ),
 .UNSPECIFIED. ) 
 CURVE ( )  GEOMETRIC_REPRESENTATION_ITEM ( )  RATIONAL_B_SPLINE_CURVE ( ( 0.9330127018922194093, 0.9330127018922196314, 1.000000000000000000, 0.8660254037844387076, 1.000000000000000000, 0.8660254037844387076, 1.000000000000000000, 0.9330127018922191873, 0.9330127018922194093 ) ) 
 REPRESENTATION_ITEM ( '' )  );
#11896 = CARTESIAN_POINT ( 'NONE',  ( 3.756430356250004099, 27.09062499938548285, 6.831223922626973533 ) ) ;
#11897 = DIRECTION ( 'NONE',  ( -0.4257792915650642218, 0.9048270524660235736, 0.000000000000000000 ) ) ;
#11898 = CARTESIAN_POINT ( 'NONE',  ( 30.12293631110040693, -7.734255490827107948, -6.500000000000000000 ) ) ;
#11899 = CARTESIAN_POINT ( 'NONE',  ( -3.999999999999996447, -8.999999999999992895, 2.925000000000000711 ) ) ;
#11900 = CARTESIAN_POINT ( 'NONE',  ( -25.45105997952899912, 17.87326343783971083, 1.000000000000000000 ) ) ;
#11901 = CARTESIAN_POINT ( 'NONE',  ( 2.000000000000000888, 25.76874999877096784, 12.46410161513774817 ) ) ;
#11902 = DIRECTION ( 'NONE',  ( 0.000000000000000000, 1.000000000000000000, 0.000000000000000000 ) ) ;
#11903 = CARTESIAN_POINT ( 'NONE',  ( 1.999999999999998224, -29.74374999877096926, 12.46410161513774639 ) ) ;
#11904 = CARTESIAN_POINT ( 'NONE',  ( -1.878215178124998497, 27.80312499938548498, 12.25316411605951927 ) ) ;
#11905 = CARTESIAN_POINT ( 'NONE',  ( 0.000000000000000000, 0.000000000000000000, 1.000000000000000000 ) ) ;
#11906 = FACE_OUTER_BOUND ( 'NONE', #16104, .T. ) ;
#11907 = CYLINDRICAL_SURFACE ( 'NONE', #556, 4.000000000000000000 ) ;
#11908 = EDGE_LOOP ( 'NONE', ( #21246, #12200, #9858 ) ) ;
#11909 = CARTESIAN_POINT ( 'NONE',  ( 3.469446951953614189E-15, 46.00000000000000000, 8.999999999999992895 ) ) ;
#11911 = ORIENTED_EDGE ( 'NONE', *, *, #7363, .T. ) ;
#11910 = CARTESIAN_POINT ( 'NONE',  ( 4.000000000000003553, -8.999999999999992895, 18.00000000000000000 ) ) ;
#11912 = EDGE_LOOP ( 'NONE', ( #989, #22466, #9771, #18345, #17864, #23821, #24690, #22183, #7479, #22217, #7968, #3528, #17654, #11412, #23176, #23180, #11760, #4762, #13508, #13482, #9833, #24685, #4333, #22531, #1834, #11587, #15809, #16134, #2524, #22533, #17777, #2778, #2976, #19255, #22397, #8486, #10051, #8940, #23301, #14345, #22671, #8007, #20572, #2115, #9224, #15362, #25589, #9706, #15988, #4059, #18591, #20803, #1735, #8130, #16750, #19090, #4128, #18376, #15780, #13438, #24554, #727, #4503, #9825, #16506, #3672, #6347, #22114, #1737, #17101, #20013, #25597, #2694, #5425, #17549, #2873, #17441, #1370, #13516, #18461, #11845, #16225, #20101, #1860, #19378, #5236, #14231, #2632, #20541, #5555, #1202, #12828, #20271, #23273, #6545, #12303, #25080, #4906, #19938, #14440, #7294, #10592, #17812, #1379, #17745, #19316, #9597, #8599, #15429, #616, #13817, #3645, #9849, #5838, #18586, #22367, #21560, #18501, #19515, #4389, #3388, #8311, #3976, #6640, #16760, #19404, #10082, #21942, #17137, #19976, #24338, #7966, #3850, #12337, #7823, #8000, #2000, #25408, #22368, #16409, #3709, #25479, #549, #22306, #11358, #793, #23922, #4971, #22468, #10266, #795, #9145, #6259, #13914, #10851, #9983, #11036, #22177, #23154, #14237, #12992, #6813, #3526, #14616, #19136, #16945, #19839, #16502, #7326, #14040, #8671, #14553, #18346, #18876, #18110, #2398, #3396, #3078, #6258, #25629, #6250, #18872, #22863, #8666, #3055, #11266, #8312, #11199, #19311, #24824, #21697, #1832, #5415, #824, #7237, #2073, #6601, #14179, #19111, #5420, #4352, #2005, #2598, #12590, #1802, #15621, #10299, #4226, #3916, #18050, #14375, #23852, #25245, #13449, #10176, #3435, #12982, #14145, #2371, #20397, #21451, #15087, #1267, #12846, #8192, #6907, #13505, #17716, #19057, #4876, #18878, #19212, #6870, #13714, #6568, #20324, #15488, #18588, #5545, #13267, #24789, #21988, #9355, #2725, #6293, #11653, #3113, #10598, #23363 ) ) ;
#11913 = DIRECTION ( 'NONE',  ( 0.000000000000000000, 0.000000000000000000, 1.000000000000000000 ) ) ;
#11914 = ORIENTED_EDGE ( 'NONE', *, *, #6041, .T. ) ;
#11915 = CARTESIAN_POINT ( 'NONE',  ( -1.878215178125000939, -29.67812499938548498, 12.25316411605952283 ) ) ;
#11916 = ORIENTED_EDGE ( 'NONE', *, *, #12700, .T. ) ;
#11917 = FACE_OUTER_BOUND ( 'NONE', #16509, .T. ) ;
#11918 = VERTEX_POINT ( 'NONE', #18668 ) ;
#11919 = CARTESIAN_POINT ( 'NONE',  ( 4.000000000000001776, 28.56249999999999645, 11.30940107675849760 ) ) ;
#11920 = CARTESIAN_POINT ( 'NONE',  ( -3.756430356249997438, 26.41562499938548569, 11.16877607737301048 ) ) ;
#11921 = EDGE_CURVE ( 'NONE', #11918, #14948, #20890, .T. ) ;
#11922 = DIRECTION ( 'NONE',  ( -1.000000000000000000, 0.000000000000000000, 0.000000000000000000 ) ) ;
#11923 = CARTESIAN_POINT ( 'NONE',  ( 0.000000000000000000, 0.000000000000000000, -6.500000000000000000 ) ) ;
#11924 = CARTESIAN_POINT ( 'NONE',  ( 22.31370212894720240, 19.65750475098775496, 12.25316411605952283 ) ) ;
#11925 = FACE_OUTER_BOUND ( 'NONE', #18230, .T. ) ;
#11926 = CARTESIAN_POINT ( 'NONE',  ( 14.98253926456319007, -27.25313774936425304, -6.500000000000000000 ) ) ;
#11927 = SHAPE_DEFINITION_REPRESENTATION ( #10689, #4483 ) ;
#11928 = CARTESIAN_POINT ( 'NONE',  ( 2.000000000000003997, 28.67500000000000426, 5.535898384862238508 ) ) ;
#11929 = CARTESIAN_POINT ( 'NONE',  ( 3.756430356250003211, -6.831223922626973533, 0.7406249993854815417 ) ) ;
#11930 = CARTESIAN_POINT ( 'NONE',  ( 30.91344420362545975, -3.401318489841207882, 1.000000000000000000 ) ) ;
#11931 = DIRECTION ( 'NONE',  ( 0.6845471059286901694, -0.7289686274214101092, 0.000000000000000000 ) ) ;
#11932 = AXIS2_PLACEMENT_3D ( 'NONE', #9539, #7971, #11889 ) ;
#11933 = ORIENTED_EDGE ( 'NONE', *, *, #19445, .T. ) ;
#11934 = VERTEX_POINT ( 'NONE', #24544 ) ;
#11935 = CARTESIAN_POINT ( 'NONE',  ( 3.756430356250004543, 26.19062499938549138, 6.831223922626973533 ) ) ;
#11936 = ORIENTED_EDGE ( 'NONE', *, *, #15233, .T. ) ;
#11937 = CARTESIAN_POINT ( 'NONE',  ( 1.859271017917182139E-15, 26.18124999877096570, 12.99999999999999289 ) ) ;
#11938 = CARTESIAN_POINT ( 'NONE',  ( -1.999999999999995781, 29.59374999877096712, 5.535898384862237620 ) ) ;
#11939 = CARTESIAN_POINT ( 'NONE',  ( -3.756430356249995661, 29.04062499938548569, 6.831223922626973533 ) ) ;
#11940 = CARTESIAN_POINT ( 'NONE',  ( -17.87326343783962201, -25.45105997952905597, -6.500000000000000000 ) ) ;
#11941 = VERTEX_POINT ( 'NONE', #2839 ) ;
#11942 = CARTESIAN_POINT ( 'NONE',  ( -16.66421332384701515, -26.25859848311253941, 1.000000000000000000 ) ) ;
#11943 = VERTEX_POINT ( 'NONE', #18799 ) ;
#11944 = CARTESIAN_POINT ( 'NONE',  ( -3.469446951953614189E-15, -30.00000000000000355, 8.999999999999992895 ) ) ;
#11945 = EDGE_CURVE ( 'NONE', #20109, #5929, #15950, .T. ) ;
#11946 = CARTESIAN_POINT ( 'NONE',  ( 1.878215178125004048, 26.11562499938548498, 5.746835883940462963 ) ) ;
#11947 = DIRECTION ( 'NONE',  ( 0.000000000000000000, 1.000000000000000000, 0.000000000000000000 ) ) ;
#11948 = CARTESIAN_POINT ( 'NONE',  ( 3.756430356250003655, -8.999999999999992895, 0.2531249993854844949 ) ) ;
#11949 = CARTESIAN_POINT ( 'NONE',  ( 0.000000000000000000, 0.000000000000000000, 19.59999999999999787 ) ) ;
#11950 = CARTESIAN_POINT ( 'NONE',  ( 6.009258394948636914E-15, 27.81250000000000711, 4.381197846482986158 ) ) ;
#11951 = EDGE_CURVE ( 'NONE', #22201, #18149, #4661, .T. ) ;
#11952 = CARTESIAN_POINT ( 'NONE',  ( -1.878215178124995832, 26.64062499938548711, 5.746835883940462963 ) ) ;
#11953 = CARTESIAN_POINT ( 'NONE',  ( 28.91604871112457076, -11.44867358849361416, -6.500000000000000000 ) ) ;
#11954 = EDGE_CURVE ( 'NONE', #16234, #962, #8010, .T. ) ;
#11955 = DIRECTION ( 'NONE',  ( 0.000000000000000000, 0.000000000000000000, -1.000000000000000000 ) ) ;
#11956 = CARTESIAN_POINT ( 'NONE',  ( -3.526711513758413297, 38.89679573513893729, 4.645898033752330569 ) ) ;
#11957 = CARTESIAN_POINT ( 'NONE',  ( 17.74838020778238246, 20.57680733252850303, 12.46410161513774639 ) ) ;
#11958 = CARTESIAN_POINT ( 'NONE',  ( 20.95908693567302450, 20.95908693567294989, 13.33755215474602984 ) ) ;
#11959 = DIRECTION ( 'NONE',  ( 1.000000000000000000, 0.000000000000000000, 0.000000000000000000 ) ) ;
#11960 = CARTESIAN_POINT ( 'NONE',  ( -1.057460391440397258E-14, 29.55624999877096926, 4.999999999999992006 ) ) ;
#11961 = CARTESIAN_POINT ( 'NONE',  ( 3.756430356249996994, -25.36562499938548498, 8.999999999999992895 ) ) ;
#11962 = CARTESIAN_POINT ( 'NONE',  ( 23.29708626209844269, 17.98469150617961887, 8.999999999999992895 ) ) ;
#11963 = ORIENTED_EDGE ( 'NONE', *, *, #9500, .T. ) ;
#11964 = CARTESIAN_POINT ( 'NONE',  ( 4.000000000000003553, 27.64374999877096784, 8.999999999999992895 ) ) ;
#11965 = CARTESIAN_POINT ( 'NONE',  ( -4.000000000000001776, -27.66249999999999787, 11.30940107675849760 ) ) ;
#11967 = ORIENTED_EDGE ( 'NONE', *, *, #12980, .T. ) ;
#11966 = CARTESIAN_POINT ( 'NONE',  ( 3.756430356250004099, 27.01562499938549067, 11.16877607737301403 ) ) ;
#11968 = CARTESIAN_POINT ( 'NONE',  ( -3.756430356249996105, 27.69062499938548072, 6.831223922626973533 ) ) ;
#11969 = DIRECTION ( 'NONE',  ( 0.9921147013144777649, -0.1253332335643050077, 0.000000000000000000 ) ) ;
#11970 = CARTESIAN_POINT ( 'NONE',  ( 19.82388608118429119, 23.96296185032701587, -6.500000000000000000 ) ) ;
#11971 = CARTESIAN_POINT ( 'NONE',  ( 3.469446951953614189E-15, -8.999999999999992895, 18.00000000000000000 ) ) ;
#11972 = ORIENTED_EDGE ( 'NONE', *, *, #19132, .T. ) ;
#11973 = ORIENTED_EDGE ( 'NONE', *, *, #4394, .T. ) ;
#11974 = CARTESIAN_POINT ( 'NONE',  ( -1.878215178125004048, -25.32812499938548356, 5.746835883940462963 ) ) ;
#11975 = CARTESIAN_POINT ( 'NONE',  ( 6.009258394948636914E-15, 29.41562499938548925, 4.662447845253954171 ) ) ;
#11976 = CARTESIAN_POINT ( 'NONE',  ( -3.756430356249996105, -6.831223922626973533, 2.578124999385481342 ) ) ;
#11977 = EDGE_CURVE ( 'NONE', #14884, #1313, #11072, .T. ) ;
#11978 = LINE ( 'NONE', #9776, #10837 ) ;
#11979 = FILL_AREA_STYLE ('',( #22052 ) ) ;
#11980 = CARTESIAN_POINT ( 'NONE',  ( -3.999999999999996447, -8.999999999999992895, 0.6749999999999984901 ) ) ;
#11981 = CARTESIAN_POINT ( 'NONE',  ( 20.74032577480890183, 20.74032577480883077, 12.99999999999999289 ) ) ;
#11982 = CARTESIAN_POINT ( 'NONE',  ( 14.54246377227358877, 27.49048467073853175, 1.000000000000000000 ) ) ;
#11983 = CARTESIAN_POINT ( 'NONE',  ( 18.07541709408115693, 18.07541709408108588, 4.999999999999992006 ) ) ;
#11984 = DIRECTION ( 'NONE',  ( 0.000000000000000000, 0.000000000000000000, -1.000000000000000000 ) ) ;
#11985 = CARTESIAN_POINT ( 'NONE',  ( 16.55507374853184999, 19.21127112649115531, 5.746835883940462963 ) ) ;
#11986 = CARTESIAN_POINT ( 'NONE',  ( 20.37793354945079471, 17.54950642470453204, 5.535898384862238508 ) ) ;
#11987 = ORIENTED_EDGE ( 'NONE', *, *, #5950, .F. ) ;
#11988 = CARTESIAN_POINT ( 'NONE',  ( -18.28012134629613783, -25.16042852506070560, -6.500000000000000000 ) ) ;
#11989 = CARTESIAN_POINT ( 'NONE',  ( 3.182002658620821212, 29.83112730774910659, 6.562149109989046103 ) ) ;
#11990 = CARTESIAN_POINT ( 'NONE',  ( 3.756430356250003655, 27.50312499938548427, 8.999999999999992895 ) ) ;
#11991 = CARTESIAN_POINT ( 'NONE',  ( -4.000096396247766251, 29.73212452601126188, 9.259737768674039415 ) ) ;
#11992 = FACE_OUTER_BOUND ( 'NONE', #12821, .T. ) ;
#11993 = CARTESIAN_POINT ( 'NONE',  ( 3.575950304376171562, 38.86679461760645182, 13.35281166003925613 ) ) ;
#11994 = ORIENTED_EDGE ( 'NONE', *, *, #15864, .T. ) ;
#11995 = CARTESIAN_POINT ( 'NONE',  ( 3.469446951953614189E-15, 30.00000000000000355, 8.999999999999992895 ) ) ;
#11996 = CARTESIAN_POINT ( 'NONE',  ( -3.999999999999996447, 26.06874999877096855, 8.999999999999992895 ) ) ;
#11997 = CARTESIAN_POINT ( 'NONE',  ( -23.64116323484209659, 20.20656826142307239, -6.500000000000000000 ) ) ;
#11999 = ORIENTED_EDGE ( 'NONE', *, *, #18697, .F. ) ;
#11998 = DIRECTION ( 'NONE',  ( 0.2486898871648653975, 0.9685831611286285225, 0.000000000000000000 ) ) ;
#12000 = ORIENTED_EDGE ( 'NONE', *, *, #25820, .T. ) ;
#12001 = VERTEX_POINT ( 'NONE', #22458 ) ;
#12002 = ORIENTED_EDGE ( 'NONE', *, *, #7581, .T. ) ;
#12003 = DIRECTION ( 'NONE',  ( 1.000000000000000000, 0.000000000000000000, 0.000000000000000000 ) ) ;
#12004 = CARTESIAN_POINT ( 'NONE',  ( 0.000000000000000000, 0.000000000000000000, 0.000000000000000000 ) ) ;
#12005 = VECTOR ( 'NONE', #14091, 1000.000000000000000 ) ;
#12006 = FILL_AREA_STYLE_COLOUR ( '', #25627 ) ;
#12007 = EDGE_CURVE ( 'NONE', #2048, #14460, #10925, .T. ) ;
#12008 = CARTESIAN_POINT ( 'NONE',  ( 1.878215178125003382, 27.46562499938548996, 5.746835883940462963 ) ) ;
#12009 = DIRECTION ( 'NONE',  ( 0.000000000000000000, 0.000000000000000000, 1.000000000000000000 ) ) ;
#12010 = CARTESIAN_POINT ( 'NONE',  ( -1.999999999999998224, -12.46410161513774639, 3.843749998770965792 ) ) ;
#12011 = CARTESIAN_POINT ( 'NONE',  ( -1.878215178124998497, 29.60312499938548569, 12.25316411605951927 ) ) ;
#12012 = ADVANCED_FACE ( 'NONE', ( #25326 ), #23234, .F. ) ;
#12013 = PLANE ( 'NONE',  #2957 ) ;
#12014 = DIRECTION ( 'NONE',  ( 0.000000000000000000, 0.000000000000000000, 1.000000000000000000 ) ) ;
#12015 = CARTESIAN_POINT ( 'NONE',  ( -3.756430356249996994, 27.16562499938548214, 8.999999999999992895 ) ) ;
#12016 = CARTESIAN_POINT ( 'NONE',  ( -3.469446951953614189E-15, -30.00000000000000355, 8.999999999999992895 ) ) ;
#12017 = CYLINDRICAL_SURFACE ( 'NONE', #11189, 0.4999999999999970024 ) ;
#12018 = DIRECTION ( 'NONE',  ( 0.000000000000000000, 0.000000000000000000, 1.000000000000000000 ) ) ;
#12019 = EDGE_CURVE ( 'NONE', #18087, #19408, #16953, .T. ) ;
#12020 = CARTESIAN_POINT ( 'NONE',  ( -2.620986760973688460E-15, -29.33124999877096784, 13.61880215351699874 ) ) ;
#12021 = CARTESIAN_POINT ( 'NONE',  ( 3.756430356250004099, 28.44062499938548783, 6.831223922626973533 ) ) ;
#12022 = DIRECTION ( 'NONE',  ( -0.000000000000000000, -0.000000000000000000, 1.000000000000000000 ) ) ;
#12023 = CIRCLE ( 'NONE', #22049, 31.10000000000000142 ) ;
#12024 = CARTESIAN_POINT ( 'NONE',  ( 17.67766952966372429, 17.67766952966365679, 8.999999999999992895 ) ) ;
#12025 = DIRECTION ( 'NONE',  ( 1.000000000000000000, 0.000000000000000000, 0.000000000000000000 ) ) ;
#12026 = ORIENTED_EDGE ( 'NONE', *, *, #15336, .F. ) ;
#12027 = EDGE_CURVE ( 'NONE', #12396, #1940, #19604, .T. ) ;
#12028 = LINE ( 'NONE', #2245, #7509 ) ;
#12030 = EDGE_LOOP ( 'NONE', ( #18562, #7225, #18882, #16010 ) ) ;
#12029 = DIRECTION ( 'NONE',  ( -0.5358267949790012086, -0.8443279255020122998, 0.000000000000000000 ) ) ;
#12031 = ORIENTED_EDGE ( 'NONE', *, *, #14100, .T. ) ;
#12032 = CARTESIAN_POINT ( 'NONE',  ( 17.28434138175965273, 20.11276850650576975, 5.535898384862237620 ) ) ;
#12034 = ORIENTED_EDGE ( 'NONE', *, *, #25399, .F. ) ;
#12033 = CIRCLE ( 'NONE', #18297, 0.5000000000000001110 ) ;
#12035 = ORIENTED_EDGE ( 'NONE', *, *, #25301, .F. ) ;
#12036 = ORIENTED_EDGE ( 'NONE', *, *, #10116, .F. ) ;
#12037 = DIRECTION ( 'NONE',  ( 0.000000000000000000, 0.000000000000000000, 1.000000000000000000 ) ) ;
#12038 = ADVANCED_FACE ( 'NONE', ( #23358 ), #3610, .F. ) ;
#12039 = VERTEX_POINT ( 'NONE', #7158 ) ;
#12040 = CARTESIAN_POINT ( 'NONE',  ( 3.469446951953614189E-15, 40.00000000000000000, 4.999999999999992006 ) ) ;
#12041 = CARTESIAN_POINT ( 'NONE',  ( 3.756430356250003655, 25.70312499938548356, 8.999999999999992895 ) ) ;
#12042 = VECTOR ( 'NONE', #17768, 999.9999999999998863 ) ;
#12043 = DIRECTION ( 'NONE',  ( -0.000000000000000000, -0.000000000000000000, 1.000000000000000000 ) ) ;
#12044 = AXIS2_PLACEMENT_3D ( 'NONE', #19925, #81, #17731 ) ;
#12045 = CARTESIAN_POINT ( 'NONE',  ( 4.000000000000001776, 25.90000000000000568, 8.999999999999992895 ) ) ;
#12046 = CARTESIAN_POINT ( 'NONE',  ( 21.38789795289476103, 16.07550319697594432, 8.999999999999992895 ) ) ;
#12047 = DIRECTION ( 'NONE',  ( 0.1873813145857330109, 0.9822872507286871668, 0.000000000000000000 ) ) ;
#12048 = CARTESIAN_POINT ( 'NONE',  ( -26.00000000000000711, 0.000000000000000000, 20.00000000000000000 ) ) ;
#12049 = VECTOR ( 'NONE', #25345, 1000.000000000000000 ) ;
#12050 = CARTESIAN_POINT ( 'NONE',  ( 3.756430356250003655, -8.999999999999992895, 1.940624999385482496 ) ) ;
#12051 = CARTESIAN_POINT ( 'NONE',  ( -3.999999999999996447, 28.82499999999999929, 8.999999999999992895 ) ) ;
#12052 = CARTESIAN_POINT ( 'NONE',  ( -1.878215178124995832, 29.34062499938548285, 5.746835883940462963 ) ) ;
#12053 = CARTESIAN_POINT ( 'NONE',  ( 4.000000000000003553, -8.999999999999992895, 3.599999999999999201 ) ) ;
#12054 = CARTESIAN_POINT ( 'NONE',  ( 20.16359180683815921, 20.16359180683808106, 4.662447845253954171 ) ) ;
#12055 = CARTESIAN_POINT ( 'NONE',  ( 3.918623196469491088, 31.50000000000000000, 13.54361004533742907 ) ) ;
#12056 = ORIENTED_EDGE ( 'NONE', *, *, #389, .T. ) ;
#12057 = ADVANCED_FACE ( 'NONE', ( #17240 ), #20766, .T. ) ;
#12058 = ORIENTED_EDGE ( 'NONE', *, *, #18638, .T. ) ;
#12059 = CARTESIAN_POINT ( 'NONE',  ( 3.756430356250004543, 26.64062499938549067, 6.831223922626973533 ) ) ;
#12060 = EDGE_CURVE ( 'NONE', #13988, #3291, #9979, .T. ) ;
#12062 = ORIENTED_EDGE ( 'NONE', *, *, #21128, .F. ) ;
#12061 = CIRCLE ( 'NONE', #2888, 0.5000000000000001110 ) ;
#12063 = CARTESIAN_POINT ( 'NONE',  ( 2.000000000000003997, 26.42500000000000071, 5.535898384862238508 ) ) ;
#12064 = CARTESIAN_POINT ( 'NONE',  ( -1.878215178124995832, 25.40312499938548640, 5.746835883940462963 ) ) ;
#12065 = CIRCLE ( 'NONE', #17861, 0.5000000000000004441 ) ;
#12066 = DIRECTION ( 'NONE',  ( 0.000000000000000000, 0.000000000000000000, 1.000000000000000000 ) ) ;
#12067 = DIRECTION ( 'NONE',  ( 0.000000000000000000, 0.000000000000000000, 1.000000000000000000 ) ) ;
#12068 = ORIENTED_EDGE ( 'NONE', *, *, #8779, .T. ) ;
#12069 = EDGE_CURVE ( 'NONE', #21212, #3297, #10436, .T. ) ;
#12070 = CIRCLE ( 'NONE', #7060, 0.5000000000000003331 ) ;
#12071 = EDGE_CURVE ( 'NONE', #17619, #8646, #20973, .T. ) ;
#12072 = CARTESIAN_POINT ( 'NONE',  ( 8.217531866531214035, 29.99470236596028982, -6.500000000000000000 ) ) ;
#12073 = CIRCLE ( 'NONE', #13744, 31.10000000000000142 ) ;
#12074 = VERTEX_POINT ( 'NONE', #2148 ) ;
#12075 = DIRECTION ( 'NONE',  ( 0.000000000000000000, 0.000000000000000000, 1.000000000000000000 ) ) ;
#12076 = CARTESIAN_POINT ( 'NONE',  ( 3.735045420075836212E-15, 26.60312499938547859, 4.662447845253954171 ) ) ;
#12077 = CARTESIAN_POINT ( 'NONE',  ( -11.44867358849309547, 28.91604871112477326, -6.500000000000000000 ) ) ;
#12078 = EDGE_CURVE ( 'NONE', #15395, #3609, #7775, .T. ) ;
#12079 = DIRECTION ( 'NONE',  ( 0.000000000000000000, 0.000000000000000000, 1.000000000000000000 ) ) ;
#12080 = LINE ( 'NONE', #22290, #14598 ) ;
#12081 = CARTESIAN_POINT ( 'NONE',  ( -3.999999999999996447, 28.82500000000000284, 8.999999999999992895 ) ) ;
#12082 = CIRCLE ( 'NONE', #12932, 31.10000000000000142 ) ;
#12083 = AXIS2_PLACEMENT_3D ( 'NONE', #14917, #21181, #9414 ) ;
#12084 = CARTESIAN_POINT ( 'NONE',  ( 3.756430356250002323, 26.00312499938548427, 11.16877607737301226 ) ) ;
#12085 = AXIS2_PLACEMENT_3D ( 'NONE', #19506, #25670, #11277 ) ;
#12086 = CARTESIAN_POINT ( 'NONE',  ( 1.071796769724487230, -28.67634618820330417, 4.999999999999992006 ) ) ;
#12087 = VECTOR ( 'NONE', #8667, 1000.000000000000000 ) ;
#12088 = CARTESIAN_POINT ( 'NONE',  ( -3.688187414285967858, 38.77776551522837423, 4.624837864698400303 ) ) ;
#12089 = DIRECTION ( 'NONE',  ( 1.000000000000000000, 0.000000000000000000, 0.000000000000000000 ) ) ;
#12090 = DIRECTION ( 'NONE',  ( 1.000000000000000000, 0.000000000000000000, 0.000000000000000000 ) ) ;
#12091 = LINE ( 'NONE', #20066, #2570 ) ;
#12092 = FACE_OUTER_BOUND ( 'NONE', #12531, .T. ) ;
#12094 = EDGE_CURVE ( 'NONE', #18284, #13049, #13783, .T. ) ;
#12093 = LINE ( 'NONE', #24002, #6637 ) ;
#12095 = CARTESIAN_POINT ( 'NONE',  ( 23.32360276639294128, 18.01120801047411391, 6.831223922626973533 ) ) ;
#12096 = AXIS2_PLACEMENT_3D ( 'NONE', #25269, #19244, #11402 ) ;
#12097 = EDGE_LOOP ( 'NONE', ( #9262, #25460 ) ) ;
#12098 = CARTESIAN_POINT ( 'NONE',  ( 4.000000000000003553, 27.68124999877096926, 6.690598923241489970 ) ) ;
#12099 = CARTESIAN_POINT ( 'NONE',  ( 1.999999999999995781, -29.19999999999999929, 5.535898384862237620 ) ) ;
#12101 = VERTEX_POINT ( 'NONE', #19794 ) ;
#12100 = CARTESIAN_POINT ( 'NONE',  ( -2.003086131649545506E-15, 26.49062499938548498, 13.33755215474603162 ) ) ;
#12102 = CARTESIAN_POINT ( 'NONE',  ( 3.735045420075836212E-15, 28.96562499938548640, 4.662447845253954171 ) ) ;
#12103 = VECTOR ( 'NONE', #17797, 1000.000000000000000 ) ;
#12104 = LINE ( 'NONE', #4125, #878 ) ;
#12105 = CARTESIAN_POINT ( 'NONE',  ( -3.756430356250002323, -29.60312499938548569, 11.16877607737301226 ) ) ;
#12106 = ORIENTED_EDGE ( 'NONE', *, *, #25028, .F. ) ;
#12107 = ORIENTED_EDGE ( 'NONE', *, *, #6708, .T. ) ;
#12108 = CARTESIAN_POINT ( 'NONE',  ( -1.878215178125000939, -25.62812499938548783, 12.25316411605952283 ) ) ;
#12109 = CARTESIAN_POINT ( 'NONE',  ( -3.756430356250000546, 26.75312499938548783, 11.16877607737301226 ) ) ;
#12110 = CARTESIAN_POINT ( 'NONE',  ( 22.03079565047434585, 16.37394140098189865, 11.30940107675849760 ) ) ;
#12111 = VECTOR ( 'NONE', #4663, 1000.000000000000000 ) ;
#12112 = EDGE_CURVE ( 'NONE', #6766, #25247, #7594, .T. ) ;
#12113 = CARTESIAN_POINT ( 'NONE',  ( 3.756430356250002323, -11.16877607737301403, 2.803124999385479654 ) ) ;
#12114 = VECTOR ( 'NONE', #7260, 1000.000000000000114 ) ;
#12115 = CARTESIAN_POINT ( 'NONE',  ( -3.999999999999995559, 27.38124999877096855, 6.690598923241487306 ) ) ;
#12116 =( LENGTH_UNIT ( ) NAMED_UNIT ( * ) SI_UNIT ( .MILLI., .METRE. ) );
#12117 = DIRECTION ( 'NONE',  ( 1.000000000000000000, 0.000000000000000000, 0.000000000000000000 ) ) ;
#12118 =( BOUNDED_CURVE ( )  B_SPLINE_CURVE ( 2, ( #8365, #16092, #19866, #17916, #7983, #6403, #15971 ),
 .UNSPECIFIED., .F., .F. ) 
 B_SPLINE_CURVE_WITH_KNOTS ( ( 3, 2, 2, 3 ),
 ( 0.1499999999999996891, 0.1666666666666665741, 0.1833333333333334592, 0.2000000000000003719 ),
 .UNSPECIFIED. ) 
 CURVE ( )  GEOMETRIC_REPRESENTATION_ITEM ( )  RATIONAL_B_SPLINE_CURVE ( ( 1.000000000000002665, 0.8660254037844363761, 1.000000000000000000, 0.8660254037844387076, 1.000000000000000000, 0.8660254037844358210, 1.000000000000002887 ) ) 
 REPRESENTATION_ITEM ( '' )  );
#12119 = AXIS2_PLACEMENT_3D ( 'NONE', #21648, #3488, #13561 ) ;
#12120 = CARTESIAN_POINT ( 'NONE',  ( 4.000000000000003553, -8.999999999999992895, 18.00000000000000000 ) ) ;
#12121 = DIRECTION ( 'NONE',  ( 0.000000000000000000, 0.000000000000000000, 1.000000000000000000 ) ) ;
#12122 = DIRECTION ( 'NONE',  ( 1.000000000000000000, 0.000000000000000000, 0.000000000000000000 ) ) ;
#12123 = CYLINDRICAL_SURFACE ( 'NONE', #14560, 4.000000000000000000 ) ;
#12124 = CARTESIAN_POINT ( 'NONE',  ( 22.66719175354224092, 17.01033750404978306, 11.30940107675849760 ) ) ;
#12125 = ORIENTED_EDGE ( 'NONE', *, *, #23050, .T. ) ;
#12126 = CARTESIAN_POINT ( 'NONE',  ( 2.900000000000003464, -8.999999999999992895, -10.00000000000000000 ) ) ;
#12127 = CARTESIAN_POINT ( 'NONE',  ( 1.500000000000001776, -10.49999999999999289, 30.00000000000000355 ) ) ;
#12128 = CARTESIAN_POINT ( 'NONE',  ( 3.756430356250003655, 25.59062499938548285, 8.999999999999992895 ) ) ;
#12129 = DIRECTION ( 'NONE',  ( 0.000000000000000000, 0.000000000000000000, 1.000000000000000000 ) ) ;
#12130 = CARTESIAN_POINT ( 'NONE',  ( 4.648177544792955347E-16, 29.33124999877097139, 12.99999999999999289 ) ) ;
#12131 = FACE_OUTER_BOUND ( 'NONE', #25303, .T. ) ;
#12132 = EDGE_LOOP ( 'NONE', ( #16328, #9740, #7195, #21382 ) ) ;
#12133 = CARTESIAN_POINT ( 'NONE',  ( -4.648177544792955347E-16, 26.85624999877096997, 4.999999999999991118 ) ) ;
#12134 = CARTESIAN_POINT ( 'NONE',  ( 4.000000000000003553, 26.33124999877097139, 6.690598923241489970 ) ) ;
#12135 = CARTESIAN_POINT ( 'NONE',  ( -3.735045420075836212E-15, -25.25312499938548783, 4.662447845253954171 ) ) ;
#12137 = VERTEX_POINT ( 'NONE', #1187 ) ;
#12136 = LINE ( 'NONE', #14494, #25027 ) ;
#12138 = AXIS2_PLACEMENT_3D ( 'NONE', #24889, #23181, #14827 ) ;
#12139 = ORIENTED_EDGE ( 'NONE', *, *, #9299, .T. ) ;
#12141 = EDGE_CURVE ( 'NONE', #3500, #13892, #17220, .T. ) ;
#12140 = ORIENTED_EDGE ( 'NONE', *, *, #7002, .T. ) ;
#12142 = PRODUCT ( 'stem', 'stem', '', ( #13163 ) ) ;
#12143 = ORIENTED_EDGE ( 'NONE', *, *, #16545, .F. ) ;
#12144 = DIRECTION ( 'NONE',  ( -0.7289686274214168815, -0.6845471059286831750, 0.000000000000000000 ) ) ;
#12145 = AXIS2_PLACEMENT_3D ( 'NONE', #15555, #23524, #5608 ) ;
#12146 = CARTESIAN_POINT ( 'NONE',  ( -1.878215178124994722, 25.40312499938548996, 5.746835883940462963 ) ) ;
#12147 = CIRCLE ( 'NONE', #15075, 0.5000000000000001110 ) ;
#12148 = VECTOR ( 'NONE', #6741, 1000.000000000000000 ) ;
#12149 = CARTESIAN_POINT ( 'NONE',  ( 3.756430356250004543, 26.00312499938548783, 11.16877607737301226 ) ) ;
#12150 = AXIS2_PLACEMENT_3D ( 'NONE', #268, #22230, #5887 ) ;
#12151 = DIRECTION ( 'NONE',  ( -1.000000000000000000, 0.000000000000000000, -0.000000000000000000 ) ) ;
#12152 = CARTESIAN_POINT ( 'NONE',  ( -3.999999999999996447, -8.999999999999992895, 3.318749998770968102 ) ) ;
#12153 = FILL_AREA_STYLE_COLOUR ( '', #13100 ) ;
#12154 = CARTESIAN_POINT ( 'NONE',  ( 3.735045420075836212E-15, 26.60312499938547859, 4.662447845253954171 ) ) ;
#12155 = CARTESIAN_POINT ( 'NONE',  ( -1.952785157361201618, 31.03863125411927371, -6.500000000000000000 ) ) ;
#12156 = CIRCLE ( 'NONE', #2983, 31.10000000000000142 ) ;
#12157 = CARTESIAN_POINT ( 'NONE',  ( -1.878215178124998497, 26.79062499938548214, 12.25316411605951927 ) ) ;
#12158 = CARTESIAN_POINT ( 'NONE',  ( 4.000000000000003553, -8.999999999999992895, 4.049999999999998046 ) ) ;
#12159 = CARTESIAN_POINT ( 'NONE',  ( -5.706339097770935176, 29.50000000000000000, 7.145898033750358813 ) ) ;
#12160 = CARTESIAN_POINT ( 'NONE',  ( -3.756430356250004099, -25.29062499938548569, 6.831223922626973533 ) ) ;
#12161 = AXIS2_PLACEMENT_3D ( 'NONE', #7019, #15005, #22986 ) ;
#12162 = CARTESIAN_POINT ( 'NONE',  ( 3.756430356250003655, 29.75312499938548783, 8.999999999999992895 ) ) ;
#12163 = CARTESIAN_POINT ( 'NONE',  ( -3.999999999999997335, 27.96250000000000213, 11.30940107675849404 ) ) ;
#12164 = CARTESIAN_POINT ( 'NONE',  ( 4.000000000000005329, 28.05624999877096926, 11.30940107675849760 ) ) ;
#12165 = CARTESIAN_POINT ( 'NONE',  ( 23.65505907007413811, 18.34266431415531073, 8.999999999999992895 ) ) ;
#12166 = ORIENTED_EDGE ( 'NONE', *, *, #24563, .T. ) ;
#12167 = CARTESIAN_POINT ( 'NONE',  ( 4.000000000000003553, 25.43124999877097281, 6.690598923241489970 ) ) ;
#12169 = VERTEX_POINT ( 'NONE', #15316 ) ;
#12168 = CARTESIAN_POINT ( 'NONE',  ( 3.999999999999972466, -6.690598923241471319, 3.581249998770966503 ) ) ;
#12170 = VECTOR ( 'NONE', #14741, 1000.000000000000000 ) ;
#12172 = ORIENTED_EDGE ( 'NONE', *, *, #15359, .F. ) ;
#12171 = EDGE_CURVE ( 'NONE', #14315, #1503, #7338, .T. ) ;
#12173 = VERTEX_POINT ( 'NONE', #5505 ) ;
#12174 = ORIENTED_EDGE ( 'NONE', *, *, #5637, .F. ) ;
#12175 = ORIENTED_EDGE ( 'NONE', *, *, #6227, .T. ) ;
#12176 = CARTESIAN_POINT ( 'NONE',  ( 0.000000000000000000, 0.000000000000000000, 17.69999999999999929 ) ) ;
#12177 = EDGE_CURVE ( 'NONE', #7296, #20975, #9281, .T. ) ;
#12178 = VECTOR ( 'NONE', #18737, 1000.000000000000000 ) ;
#12179 = ORIENTED_EDGE ( 'NONE', *, *, #8568, .T. ) ;
#12180 = ADVANCED_FACE ( 'NONE', ( #7215 ), #5368, .F. ) ;
#12181 = CARTESIAN_POINT ( 'NONE',  ( 4.000000000000003553, 29.50000000000000355, 8.999999999999992895 ) ) ;
#12182 = CARTESIAN_POINT ( 'NONE',  ( 3.735045420075836212E-15, 26.26562499938548356, 4.662447845253954171 ) ) ;
#12183 = VECTOR ( 'NONE', #6507, 1000.000000000000000 ) ;
#12184 = VECTOR ( 'NONE', #21201, 1000.000000000000000 ) ;
#12185 = CARTESIAN_POINT ( 'NONE',  ( -3.756430356249997882, -11.16877607737301226, 1.865624999385482985 ) ) ;
#12186 = CARTESIAN_POINT ( 'NONE',  ( -0.5000000000000000000, 6.000000000000000000, 19.50000000000000000 ) ) ;
#12187 = CARTESIAN_POINT ( 'NONE',  ( 19.60674521665374215, 19.60674521665367820, 13.33755215474602984 ) ) ;
#12188 = EDGE_CURVE ( 'NONE', #14283, #17328, #8619, .T. ) ;
#12189 = AXIS2_PLACEMENT_3D ( 'NONE', #11218, #23646, #19339 ) ;
#12190 = LINE ( 'NONE', #8265, #6306 ) ;
#12191 = FACE_OUTER_BOUND ( 'NONE', #11270, .T. ) ;
#12192 = ITEM_DEFINED_TRANSFORMATION ( 'NONE', 'NONE', #4351,  #21036 ) ;
#12193 = CARTESIAN_POINT ( 'NONE',  ( -3.756430356249997882, -11.16877607737301226, 2.203124999385479565 ) ) ;
#12194 = CARTESIAN_POINT ( 'NONE',  ( -1.999999999999998224, 28.84374999877097423, 12.46410161513774639 ) ) ;
#12195 = CARTESIAN_POINT ( 'NONE',  ( 3.878215178125003604, -8.999999999999992895, 4.570312499692741781 ) ) ;
#12196 = DIRECTION ( 'NONE',  ( 0.000000000000000000, 0.000000000000000000, 1.000000000000000000 ) ) ;
#12197 = LINE ( 'NONE', #10486, #10931 ) ;
#12198 = CARTESIAN_POINT ( 'NONE',  ( 2.000000000000000888, 27.56874999877096855, 12.46410161513774817 ) ) ;
#12199 = AXIS2_PLACEMENT_3D ( 'NONE', #19092, #23275, #7585 ) ;
#12200 = ORIENTED_EDGE ( 'NONE', *, *, #13246, .F. ) ;
#12201 = EDGE_LOOP ( 'NONE', ( #24577, #25717, #23879, #15210 ) ) ;
#12202 = CARTESIAN_POINT ( 'NONE',  ( -3.756430356249996105, 26.34062499938548285, 6.831223922626973533 ) ) ;
#12203 = VECTOR ( 'NONE', #21426, 1000.000000000000000 ) ;
#12204 = VECTOR ( 'NONE', #4959, 1000.000000000000000 ) ;
#12205 = ORIENTED_EDGE ( 'NONE', *, *, #6465, .T. ) ;
#12206 = CARTESIAN_POINT ( 'NONE',  ( -30.54913349766215802, 5.827558883616378083, -6.500000000000000000 ) ) ;
#12207 = VERTEX_POINT ( 'NONE', #25258 ) ;
#12208 = DIRECTION ( 'NONE',  ( 3.552713678800501718E-15, 0.000000000000000000, 1.000000000000000000 ) ) ;
#12209 = VERTEX_POINT ( 'NONE', #13358 ) ;
#12210 = VECTOR ( 'NONE', #24421, 1000.000000000000000 ) ;
#12211 = EDGE_CURVE ( 'NONE', #8412, #24490, #19364, .T. ) ;
#12212 = LINE ( 'NONE', #5941, #7356 ) ;
#12213 = ORIENTED_EDGE ( 'NONE', *, *, #15240, .T. ) ;
#12214 = DIRECTION ( 'NONE',  ( -0.7071067811865487940, -0.7071067811865463515, 0.000000000000000000 ) ) ;
#12215 = CARTESIAN_POINT ( 'NONE',  ( 2.672651547586948120E-15, 26.82812499938548356, 13.33755215474602984 ) ) ;
#12216 = CARTESIAN_POINT ( 'NONE',  ( 0.000000000000000000, 0.000000000000000000, -6.500000000000000000 ) ) ;
#12217 = AXIS2_PLACEMENT_3D ( 'NONE', #23373, #17371, #13188 ) ;
#12218 = CARTESIAN_POINT ( 'NONE',  ( 1.071796769724492338, 26.70759618943233704, 12.99999999999999467 ) ) ;
#12219 = DIRECTION ( 'NONE',  ( 1.000000000000000000, 0.000000000000000000, 0.000000000000000000 ) ) ;
#12220 = CARTESIAN_POINT ( 'NONE',  ( 4.000000000000002665, 29.01250000000000284, 11.30940107675849760 ) ) ;
#12221 = EDGE_CURVE ( 'NONE', #1657, #25409, #23284, .T. ) ;
#12222 = EDGE_CURVE ( 'NONE', #3647, #20357, #3428, .T. ) ;
#12223 = CARTESIAN_POINT ( 'NONE',  ( -3.756430356249997882, 25.40312499938548285, 11.16877607737301226 ) ) ;
#12224 = DIRECTION ( 'NONE',  ( 1.000000000000000000, 0.000000000000000000, 0.000000000000000000 ) ) ;
#12225 = AXIS2_PLACEMENT_3D ( 'NONE', #14954, #9196, #4884 ) ;
#12226 = CARTESIAN_POINT ( 'NONE',  ( -4.000000000000021316, -11.30940107675847806, 2.062499999999996891 ) ) ;
#12227 = DIRECTION ( 'NONE',  ( -0.000000000000000000, -0.000000000000000000, 1.000000000000000000 ) ) ;
#12228 = CARTESIAN_POINT ( 'NONE',  ( 3.110308778861319734, 31.50000000000000000, 3.869115154270335477 ) ) ;
#12229 = CARTESIAN_POINT ( 'NONE',  ( 21.54465973840859760, 18.71623261366233848, 12.46410161513774817 ) ) ;
#12230 = CARTESIAN_POINT ( 'NONE',  ( -2.672651547586948120E-15, -25.92812499938548498, 13.33755215474603162 ) ) ;
#12231 = CARTESIAN_POINT ( 'NONE',  ( -1.999999999999998224, -12.46410161513774639, 0.3000000000000016542 ) ) ;
#12232 = ORIENTED_EDGE ( 'NONE', *, *, #1567, .F. ) ;
#12233 = CARTESIAN_POINT ( 'NONE',  ( 2.000000000000003997, 27.26874999877097139, 5.535898384862238508 ) ) ;
#12234 = CARTESIAN_POINT ( 'NONE',  ( -9.110428525060477511, 29.57785765677940404, -6.500000000000000000 ) ) ;
#12236 = ORIENTED_EDGE ( 'NONE', *, *, #22026, .F. ) ;
#12235 = CARTESIAN_POINT ( 'NONE',  ( -3.756430356249997882, 27.24062499938548854, 6.831223922626973533 ) ) ;
#12237 = VERTEX_POINT ( 'NONE', #13613 ) ;
#12238 = CARTESIAN_POINT ( 'NONE',  ( 1.878215178125004048, 28.47812499938548569, 5.746835883940462963 ) ) ;
#12239 = CYLINDRICAL_SURFACE ( 'NONE', #1287, 0.5000000000000004441 ) ;
#12240 = PLANE ( 'NONE',  #17563 ) ;
#12241 = ORIENTED_EDGE ( 'NONE', *, *, #21784, .F. ) ;
#12242 = ORIENTED_EDGE ( 'NONE', *, *, #2578, .T. ) ;
#12243 = CARTESIAN_POINT ( 'NONE',  ( -3.756430356250003211, -26.19062499938548783, 6.831223922626973533 ) ) ;
#12244 = CARTESIAN_POINT ( 'NONE',  ( -3.756430356249996105, 29.00312499938548427, 11.16877607737301226 ) ) ;
#12245 = CARTESIAN_POINT ( 'NONE',  ( 1.626862140677534194E-14, 27.98124999877096997, 12.99999999999999289 ) ) ;
#12246 = EDGE_CURVE ( 'NONE', #16230, #24819, #11513, .T. ) ;
#12247 = CARTESIAN_POINT ( 'NONE',  ( 3.756430356250003655, -8.999999999999992895, 3.740624999385481875 ) ) ;
#12248 = VECTOR ( 'NONE', #19687, 1000.000000000000000 ) ;
#12249 = EDGE_CURVE ( 'NONE', #13593, #702, #17411, .T. ) ;
#12250 = AXIS2_PLACEMENT_3D ( 'NONE', #6366, #4659, #16567 ) ;
#12251 = CARTESIAN_POINT ( 'NONE',  ( -3.999999999999996447, -8.999999999999992895, 3.374999999999999556 ) ) ;
#12252 = PRESENTATION_STYLE_ASSIGNMENT (( #14085 ) ) ;
#12253 = DIRECTION ( 'NONE',  ( 0.000000000000000000, 0.000000000000000000, 1.000000000000000000 ) ) ;
#12254 = CARTESIAN_POINT ( 'NONE',  ( 3.401318489841097747, 30.91344420362547396, 1.000000000000000000 ) ) ;
#12255 = CARTESIAN_POINT ( 'NONE',  ( 30.24338421796779386, -7.248980000274303670, -2.750000000000000000 ) ) ;
#12256 = CARTESIAN_POINT ( 'NONE',  ( 1.000000000000000000, 0.000000000000000000, 20.00000000000000000 ) ) ;
#12257 = CARTESIAN_POINT ( 'NONE',  ( -1.071796769724485232, 26.42634618820330772, 4.999999999999992006 ) ) ;
#12258 = CARTESIAN_POINT ( 'NONE',  ( 18.81125008781888042, 18.81125008781880581, 4.662447845253954171 ) ) ;
#12259 = CARTESIAN_POINT ( 'NONE',  ( 23.01190630937068349, 17.35505205987822919, 8.999999999999992895 ) ) ;
#12260 = ORIENTED_EDGE ( 'NONE', *, *, #17375, .T. ) ;
#12261 = DIRECTION ( 'NONE',  ( -2.891205793294678326E-16, -1.000000000000000000, 0.000000000000000000 ) ) ;
#12262 = CARTESIAN_POINT ( 'NONE',  ( -1.878215178124998497, 29.15312499938548640, 12.25316411605951927 ) ) ;
#12264 = VERTEX_POINT ( 'NONE', #5633 ) ;
#12263 = FACE_OUTER_BOUND ( 'NONE', #5769, .T. ) ;
#12265 = COLOUR_RGB ( '',0.8941176470588234615, 0.8941176470588234615, 0.8941176470588234615 ) ;
#12266 = CARTESIAN_POINT ( 'NONE',  ( 4.648177544792954952E-15, 25.73124999877097707, 12.99999999999999289 ) ) ;
#12267 = LINE ( 'NONE', #2212, #24245 ) ;
#12268 = ORIENTED_EDGE ( 'NONE', *, *, #24499, .F. ) ;
#12269 = CARTESIAN_POINT ( 'NONE',  ( 0.4995657836784155315, 31.50000000000000000, 3.020833333333325044 ) ) ;
#12270 = CARTESIAN_POINT ( 'NONE',  ( 2.000000000000000888, 25.76874999877096784, 12.46410161513774817 ) ) ;
#12271 = CARTESIAN_POINT ( 'NONE',  ( -1.878215178125000939, -26.41562499938548214, 12.25316411605952283 ) ) ;
#12273 = ORIENTED_EDGE ( 'NONE', *, *, #20173, .T. ) ;
#12272 = FACE_OUTER_BOUND ( 'NONE', #5620, .T. ) ;
#12274 = AXIS2_PLACEMENT_3D ( 'NONE', #9479, #17457, #15368 ) ;
#12275 = VERTEX_POINT ( 'NONE', #1577 ) ;
#12276 = VERTEX_POINT ( 'NONE', #7598 ) ;
#12277 = APPLICATION_CONTEXT ( 'automotive_design' ) ;
#12278 = ORIENTED_EDGE ( 'NONE', *, *, #21544, .T. ) ;
#12279 = CYLINDRICAL_SURFACE ( 'NONE', #3024, 31.10000000000000142 ) ;
#12280 =( BOUNDED_CURVE ( )  B_SPLINE_CURVE ( 2, ( #6113, #18277, #20229, #8335, #365, #14096, #22061, #4148, #9903 ),
 .UNSPECIFIED., .F., .F. ) 
 B_SPLINE_CURVE_WITH_KNOTS ( ( 3, 2, 2, 2, 3 ),
 ( 0.4250000000000000444, 0.4333333333333333481, 0.4500000000000000111, 0.4666666666666666741, 0.4750000000000000333 ),
 .UNSPECIFIED. ) 
 CURVE ( )  GEOMETRIC_REPRESENTATION_ITEM ( )  RATIONAL_B_SPLINE_CURVE ( ( 0.9330127018922194093, 0.9330127018922196314, 1.000000000000000000, 0.8660254037844387076, 1.000000000000000000, 0.8660254037844387076, 1.000000000000000000, 0.9330127018922191873, 0.9330127018922194093 ) ) 
 REPRESENTATION_ITEM ( '' )  );
#12281 = CARTESIAN_POINT ( 'NONE',  ( -3.756430356249996105, 25.96562499938548996, 11.16877607737301226 ) ) ;
#12282 = CARTESIAN_POINT ( 'NONE',  ( 4.393401135980900207, -30.78811501957146390, 1.000000000000000000 ) ) ;
#12283 = ADVANCED_FACE ( 'NONE', ( #15583 ), #21579, .F. ) ;
#12284 =( BOUNDED_CURVE ( )  B_SPLINE_CURVE ( 2, ( #25624, #15948, #21690, #3776, #17393, #25490, #23778, #11755, #25743 ),
 .UNSPECIFIED., .F., .F. ) 
 B_SPLINE_CURVE_WITH_KNOTS ( ( 3, 2, 2, 2, 3 ),
 ( 0.2250000000000000056, 0.2333333333333333370, 0.2500000000000000000, 0.2666666666666666630, 0.2750000000000000222 ),
 .UNSPECIFIED. ) 
 CURVE ( )  GEOMETRIC_REPRESENTATION_ITEM ( )  RATIONAL_B_SPLINE_CURVE ( ( 0.9330127018922194093, 0.9330127018922194093, 1.000000000000000000, 0.8660254037844387076, 1.000000000000000000, 0.8660254037844387076, 1.000000000000000000, 0.9330127018922191873, 0.9330127018922194093 ) ) 
 REPRESENTATION_ITEM ( '' )  );
#12285 = DIRECTION ( 'NONE',  ( 1.387778780781445044E-14, 1.000000000000000000, 0.000000000000000000 ) ) ;
#12286 = CARTESIAN_POINT ( 'NONE',  ( 1.878215178125000939, -12.25316411605952283, 0.6281249993854848279 ) ) ;
#12287 = CARTESIAN_POINT ( 'NONE',  ( 1.878215178125004048, 27.01562499938548711, 5.746835883940462963 ) ) ;
#12288 = EDGE_CURVE ( 'NONE', #13585, #14795, #15129, .T. ) ;
#12289 = DIRECTION ( 'NONE',  ( 1.000000000000000000, 0.000000000000000000, -0.000000000000000000 ) ) ;
#12290 = CARTESIAN_POINT ( 'NONE',  ( -3.999999999999959144, -11.30940107675851891, 1.556249998770965925 ) ) ;
#12291 = CARTESIAN_POINT ( 'NONE',  ( -1.878215178124995832, 26.19062499938548427, 5.746835883940462963 ) ) ;
#12292 = CARTESIAN_POINT ( 'NONE',  ( -0.4999838450258491940, -31.09598070739550124, 1.000000000000000000 ) ) ;
#12293 = PLANE ( 'NONE',  #9514 ) ;
#12294 = CARTESIAN_POINT ( 'NONE',  ( -1.878215178125000939, -25.62812499938548783, 12.25316411605952283 ) ) ;
#12295 = DIRECTION ( 'NONE',  ( 0.000000000000000000, 0.000000000000000000, -1.000000000000000000 ) ) ;
#12297 = EDGE_CURVE ( 'NONE', #13450, #15016, #11124, .T. ) ;
#12296 = LINE ( 'NONE', #20001, #23727 ) ;
#12298 = CARTESIAN_POINT ( 'NONE',  ( 1.533898589781675205E-14, 27.98124999877097352, 12.99999999999999289 ) ) ;
#12299 = DIRECTION ( 'NONE',  ( 0.7071067811865463515, -0.7071067811865487940, 0.000000000000000000 ) ) ;
#12300 = ORIENTED_EDGE ( 'NONE', *, *, #2589, .F. ) ;
#12301 = CYLINDRICAL_SURFACE ( 'NONE', #22126, 4.000000000000000000 ) ;
#12303 = ORIENTED_EDGE ( 'NONE', *, *, #11945, .T. ) ;
#12302 = PLANE ( 'NONE',  #22941 ) ;
#12304 = ORIENTED_EDGE ( 'NONE', *, *, #9853, .T. ) ;
#12305 = FACE_OUTER_BOUND ( 'NONE', #23058, .T. ) ;
#12306 = ORIENTED_EDGE ( 'NONE', *, *, #24265, .F. ) ;
#12307 = ORIENTED_EDGE ( 'NONE', *, *, #10752, .T. ) ;
#12308 = VERTEX_POINT ( 'NONE', #3795 ) ;
#12309 = ORIENTED_EDGE ( 'NONE', *, *, #10863, .F. ) ;
#12310 = CARTESIAN_POINT ( 'NONE',  ( 3.752267015613588906E-15, -4.381197846482986158, 2.756249998770968546 ) ) ;
#12311 = VERTEX_POINT ( 'NONE', #20131 ) ;
#12312 = DIRECTION ( 'NONE',  ( 0.000000000000000000, 1.000000000000000000, 0.000000000000000000 ) ) ;
#12313 = CARTESIAN_POINT ( 'NONE',  ( -3.756430356249997438, 27.31562499938548427, 11.16877607737301048 ) ) ;
#12314 = CARTESIAN_POINT ( 'NONE',  ( 2.672651547586948120E-15, -13.33755215474602984, 2.840624999385484184 ) ) ;
#12315 = DIRECTION ( 'NONE',  ( 0.000000000000000000, 0.000000000000000000, 1.000000000000000000 ) ) ;
#12316 = CARTESIAN_POINT ( 'NONE',  ( 16.52628376998245230, 21.83867852590112690, 6.831223922626973533 ) ) ;
#12317 = DIRECTION ( 'NONE',  ( 1.000000000000000000, 0.000000000000000000, 0.000000000000000000 ) ) ;
#12318 = EDGE_CURVE ( 'NONE', #20735, #19181, #24813, .T. ) ;
#12319 = DIRECTION ( 'NONE',  ( 0.000000000000000000, 0.000000000000000000, 1.000000000000000000 ) ) ;
#12320 = CONTEXT_DEPENDENT_SHAPE_REPRESENTATION ( #1579, #17406 ) ;
#12321 = CARTESIAN_POINT ( 'NONE',  ( 3.735045420075836212E-15, -4.662447845253954171, 2.503124999385483385 ) ) ;
#12322 = CARTESIAN_POINT ( 'NONE',  ( -5.335677986745010593, -30.63887302793242284, -6.500000000000000000 ) ) ;
#12323 = CARTESIAN_POINT ( 'NONE',  ( 3.756430356250003211, 29.22812499938548569, 6.831223922626973533 ) ) ;
#12324 = CARTESIAN_POINT ( 'NONE',  ( -3.756430356249996994, -8.999999999999992895, 1.828124999385484450 ) ) ;
#12325 = EDGE_CURVE ( 'NONE', #16191, #10388, #24305, .T. ) ;
#12326 = CARTESIAN_POINT ( 'NONE',  ( 0.000000000000000000, 0.000000000000000000, 1.000000000000000000 ) ) ;
#12327 = CARTESIAN_POINT ( 'NONE',  ( 7.734255490827002255, 30.12293631110042469, -6.500000000000000000 ) ) ;
#12328 = ADVANCED_FACE ( 'NONE', ( #19753 ), #13872, .F. ) ;
#12329 = ORIENTED_EDGE ( 'NONE', *, *, #1536, .T. ) ;
#12330 = ORIENTED_EDGE ( 'NONE', *, *, #9035, .F. ) ;
#12331 = CARTESIAN_POINT ( 'NONE',  ( 2.003086131649545506E-15, 26.94062499938549138, 13.33755215474602984 ) ) ;
#12332 = ORIENTED_EDGE ( 'NONE', *, *, #22807, .T. ) ;
#12333 = CYLINDRICAL_SURFACE ( 'NONE', #1609, 0.5000000000000004441 ) ;
#12334 = EDGE_LOOP ( 'NONE', ( #24043, #2724, #3557, #21115 ) ) ;
#12335 = CARTESIAN_POINT ( 'NONE',  ( 20.05973549791684718, 17.23130837317058806, 5.535898384862238508 ) ) ;
#12336 = EDGE_CURVE ( 'NONE', #12422, #2907, #269, .T. ) ;
#12337 = ORIENTED_EDGE ( 'NONE', *, *, #25360, .F. ) ;
#12338 = CIRCLE ( 'NONE', #12754, 31.10000000000000142 ) ;
#12339 = DIRECTION ( 'NONE',  ( 1.000000000000000000, 0.000000000000000000, 0.000000000000000000 ) ) ;
#12340 = VERTEX_POINT ( 'NONE', #18064 ) ;
#12341 = AXIS2_PLACEMENT_3D ( 'NONE', #24473, #18469, #10603 ) ;
#12342 = DIRECTION ( 'NONE',  ( 0.000000000000000000, 1.000000000000000000, 0.000000000000000000 ) ) ;
#12343 = CARTESIAN_POINT ( 'NONE',  ( -3.756430356249996994, 27.16562499938548214, 8.999999999999992895 ) ) ;
#12344 = DIRECTION ( 'NONE',  ( 0.000000000000000000, 0.000000000000000000, 1.000000000000000000 ) ) ;
#12345 = CARTESIAN_POINT ( 'NONE',  ( 7.248980000273979485, -30.24338421796786847, -6.500000000000000000 ) ) ;
#12346 = DIRECTION ( 'NONE',  ( 0.000000000000000000, 0.000000000000000000, 1.000000000000000000 ) ) ;
#12347 = EDGE_CURVE ( 'NONE', #21476, #8528, #2353, .T. ) ;
#12348 = CYLINDRICAL_SURFACE ( 'NONE', #22694, 0.5000000000000004441 ) ;
#12349 = AXIS2_PLACEMENT_3D ( 'NONE', #9223, #11438, #7645 ) ;
#12350 = CARTESIAN_POINT ( 'NONE',  ( 2.672651547586948120E-15, 27.72812499938548569, 13.33755215474602984 ) ) ;
#12351 = CARTESIAN_POINT ( 'NONE',  ( 3.834746474454188013E-15, 26.01249999999999574, 4.999999999999992006 ) ) ;
#12352 = CARTESIAN_POINT ( 'NONE',  ( 2.006336132164985451E-12, 39.00000000001113420, 3.500000000010202061 ) ) ;
#12353 = ADVANCED_FACE ( 'NONE', ( #24324 ), #3929, .F. ) ;
#12354 = CARTESIAN_POINT ( 'NONE',  ( -3.999999999999998224, 25.61874999877097281, 8.999999999999992895 ) ) ;
#12355 = DIRECTION ( 'NONE',  ( 0.000000000000000000, 0.000000000000000000, -1.000000000000000000 ) ) ;
#12356 = CARTESIAN_POINT ( 'NONE',  ( 1.878215178124995832, -25.29062499938548569, 5.746835883940462963 ) ) ;
#12357 = CARTESIAN_POINT ( 'NONE',  ( -30.60000000000000142, 3.257552089140643357E-13, 1.000000000000000000 ) ) ;
#12358 = ORIENTED_EDGE ( 'NONE', *, *, #3927, .F. ) ;
#12359 = CARTESIAN_POINT ( 'NONE',  ( 3.752267015613588906E-15, 27.75624999877096855, 4.381197846482986158 ) ) ;
#12360 = CARTESIAN_POINT ( 'NONE',  ( 3.999999999999997335, -28.41249999999999787, 11.30940107675849404 ) ) ;
#12361 = ADVANCED_FACE ( 'NONE', ( #4178 ), #19991, .T. ) ;
#12363 = ORIENTED_EDGE ( 'NONE', *, *, #8016, .F. ) ;
#12362 = CARTESIAN_POINT ( 'NONE',  ( 1.878215178125001605, 26.52812499938548640, 12.25316411605952283 ) ) ;
#12364 = VERTEX_POINT ( 'NONE', #17795 ) ;
#12365 = FACE_OUTER_BOUND ( 'NONE', #16654, .T. ) ;
#12366 = EDGE_CURVE ( 'NONE', #4853, #89, #5501, .T. ) ;
#12367 = CARTESIAN_POINT ( 'NONE',  ( 3.688104818422799358, 38.77776441442690469, 4.624767765505003680 ) ) ;
#12368 = DIRECTION ( 'NONE',  ( 0.000000000000000000, 1.000000000000000000, 0.000000000000000000 ) ) ;
#12369 = ORIENTED_EDGE ( 'NONE', *, *, #8373, .F. ) ;
#12370 = ORIENTED_EDGE ( 'NONE', *, *, #4735, .T. ) ;
#12371 = CARTESIAN_POINT ( 'NONE',  ( -3.756430356250003655, -27.50312499938548427, 8.999999999999992895 ) ) ;
#12372 = CARTESIAN_POINT ( 'NONE',  ( 0.000000000000000000, 27.72812499938548925, 13.33755215474602984 ) ) ;
#12373 = DIRECTION ( 'NONE',  ( 1.000000000000000000, 0.000000000000000000, 0.000000000000000000 ) ) ;
#12374 = CARTESIAN_POINT ( 'NONE',  ( 3.756430356250003655, -8.999999999999992895, 4.640624999385483562 ) ) ;
#12375 = DIRECTION ( 'NONE',  ( 0.8090169943749532244, 0.5877852522924652545, 0.000000000000000000 ) ) ;
#12376 = SHAPE_REPRESENTATION_RELATIONSHIP ( 'NONE' , 'NONE' ,  #13517, #21253 ) ;
#12377 = CARTESIAN_POINT ( 'NONE',  ( 12.78762572734057024, 28.34936733434201273, 1.000000000000000000 ) ) ;
#12378 = DIRECTION ( 'NONE',  ( -0.4817536741017198754, -0.8763066800438610304, 0.000000000000000000 ) ) ;
#12379 = DIRECTION ( 'NONE',  ( 1.000000000000000000, 0.000000000000000000, 0.000000000000000000 ) ) ;
#12380 = FACE_OUTER_BOUND ( 'NONE', #25274, .T. ) ;
#12381 = CARTESIAN_POINT ( 'NONE',  ( 16.84448182151639628, 22.15687657743507089, 6.831223922626973533 ) ) ;
#12382 = CARTESIAN_POINT ( 'NONE',  ( 21.65072575558658130, 18.82229863084031507, 5.535898384862238508 ) ) ;
#12383 = CARTESIAN_POINT ( 'NONE',  ( -29.07785765677917311, 9.610428525061202265, 1.000000000000000000 ) ) ;
#12384 = CARTESIAN_POINT ( 'NONE',  ( 0.000000000000000000, 0.000000000000000000, 16.00000000000000000 ) ) ;
#12385 = CARTESIAN_POINT ( 'NONE',  ( -1.878215178124998497, 26.34062499938548285, 12.25316411605951927 ) ) ;
#12387 = ORIENTED_EDGE ( 'NONE', *, *, #5782, .T. ) ;
#12386 = CARTESIAN_POINT ( 'NONE',  ( -0.5247320085691752345, 29.99650235037416834, 5.025996973432255821 ) ) ;
#12388 = CARTESIAN_POINT ( 'NONE',  ( 15.59820611967510295, 20.91060087559377934, 8.999999999999992895 ) ) ;
#12389 = CARTESIAN_POINT ( 'NONE',  ( 2.000000000000000888, -12.46410161513774817, 1.274999999999998357 ) ) ;
#12390 = ORIENTED_EDGE ( 'NONE', *, *, #3063, .F. ) ;
#12391 = CARTESIAN_POINT ( 'NONE',  ( -22.32573188046936252, -21.65113613650319380, 1.000000000000000000 ) ) ;
#12392 = DIRECTION ( 'NONE',  ( -0.000000000000000000, -1.000000000000000000, -0.000000000000000000 ) ) ;
#12393 = CARTESIAN_POINT ( 'NONE',  ( 1.878215178124998497, -26.34062499938548285, 12.25316411605951927 ) ) ;
#12394 = EDGE_CURVE ( 'NONE', #12847, #10226, #12118, .T. ) ;
#12396 = VERTEX_POINT ( 'NONE', #14000 ) ;
#12395 = CARTESIAN_POINT ( 'NONE',  ( 3.469446951953614189E-15, 40.00000000000000000, 8.999999999999992895 ) ) ;
#12397 = EDGE_CURVE ( 'NONE', #1315, #7103, #19291, .T. ) ;
#12398 = ORIENTED_EDGE ( 'NONE', *, *, #19243, .F. ) ;
#12399 = CARTESIAN_POINT ( 'NONE',  ( 1.878215178124998497, -25.89062499938548356, 12.25316411605951927 ) ) ;
#12400 = ORIENTED_EDGE ( 'NONE', *, *, #10116, .T. ) ;
#12401 = ORIENTED_EDGE ( 'NONE', *, *, #9329, .T. ) ;
#12402 = ADVANCED_FACE ( 'NONE', ( #14394 ), #22231, .T. ) ;
#12403 = CARTESIAN_POINT ( 'NONE',  ( 4.006172263299091013E-15, 25.36562499938549564, 4.662447845253954171 ) ) ;
#12404 = CARTESIAN_POINT ( 'NONE',  ( 3.834746474454188013E-15, 27.81249999999999645, 4.999999999999992006 ) ) ;
#12405 = CARTESIAN_POINT ( 'NONE',  ( 3.735045420075836212E-15, -4.662447845253954171, 1.715624999385482852 ) ) ;
#12406 =( NAMED_UNIT ( * ) PLANE_ANGLE_UNIT ( ) SI_UNIT ( $, .RADIAN. ) );
#12407 = CARTESIAN_POINT ( 'NONE',  ( 3.756430356250003655, 26.94062499938548427, 8.999999999999992895 ) ) ;
#12408 = CARTESIAN_POINT ( 'NONE',  ( 20.62100150635272300, 20.62100150635266260, 4.999999999999992006 ) ) ;
#12409 = CARTESIAN_POINT ( 'NONE',  ( -17.78012134629558716, 25.16042852506110705, 1.000000000000000000 ) ) ;
#12410 = CARTESIAN_POINT ( 'NONE',  ( 1.878215178125000939, 25.96562499938548285, 12.25316411605952283 ) ) ;
#12411 = CARTESIAN_POINT ( 'NONE',  ( -10.08469938919458286, 29.41953157733104263, 1.000000000000000000 ) ) ;
#12412 = LINE ( 'NONE', #10579, #17054 ) ;
#12413 = DIRECTION ( 'NONE',  ( -0.000000000000000000, -0.000000000000000000, -1.000000000000000000 ) ) ;
#12414 = CARTESIAN_POINT ( 'NONE',  ( -4.000000000000003553, -28.58124999877096784, 6.690598923241489970 ) ) ;
#12415 = CARTESIAN_POINT ( 'NONE',  ( -3.999999999999999112, 27.51250000000000995, 11.30940107675849404 ) ) ;
#12416 = DIRECTION ( 'NONE',  ( 0.000000000000000000, 0.000000000000000000, 1.000000000000000000 ) ) ;
#12417 = DIRECTION ( 'NONE',  ( 1.000000000000000000, 0.000000000000000000, 0.000000000000000000 ) ) ;
#12418 = CARTESIAN_POINT ( 'NONE',  ( 1.036406108997123487, -29.98318460927812268, 5.127803451112008304 ) ) ;
#12419 = ORIENTED_EDGE ( 'NONE', *, *, #10240, .F. ) ;
#12420 = CARTESIAN_POINT ( 'NONE',  ( -5.327558883615603591, 30.54913349766230724, -6.500000000000000000 ) ) ;
#12422 = VERTEX_POINT ( 'NONE', #10064 ) ;
#12421 = CYLINDRICAL_SURFACE ( 'NONE', #19584, 31.10000000000000142 ) ;
#12423 =( BOUNDED_CURVE ( )  B_SPLINE_CURVE ( 2, ( #12298, #155, #13745, #12164, #5896, #10073, #18074, #14133, #8125 ),
 .UNSPECIFIED., .F., .T. ) 
 B_SPLINE_CURVE_WITH_KNOTS ( ( 3, 2, 2, 2, 3 ),
 ( 0.5750000000000000666, 0.5833333333333333703, 0.5999999999999999778, 0.6166666666666666963, 0.6250000000000000000 ),
 .UNSPECIFIED. ) 
 CURVE ( )  GEOMETRIC_REPRESENTATION_ITEM ( )  RATIONAL_B_SPLINE_CURVE ( ( 0.9330127018922194093, 0.9330127018922198534, 1.000000000000000000, 0.8660254037844387076, 1.000000000000000000, 0.8660254037844387076, 1.000000000000000000, 0.9330127018922194093, 0.9330127018922194093 ) ) 
 REPRESENTATION_ITEM ( '' )  );
#12424 = EDGE_CURVE ( 'NONE', #15870, #6150, #146, .T. ) ;
#12425 = ORIENTED_EDGE ( 'NONE', *, *, #642, .F. ) ;
#12426 = EDGE_LOOP ( 'NONE', ( #19934, #16133, #12599, #697, #2391, #17096, #6845, #17575, #16197, #20822, #5675, #10882, #18906, #1600, #16196, #13404, #15691, #17578, #17140, #589, #19351, #16467, #6068, #19722, #1312 ) ) ;
#12427 = ORIENTED_EDGE ( 'NONE', *, *, #8266, .F. ) ;
#12428 = ORIENTED_EDGE ( 'NONE', *, *, #19709, .F. ) ;
#12429 = ORIENTED_EDGE ( 'NONE', *, *, #9891, .T. ) ;
#12430 = CARTESIAN_POINT ( 'NONE',  ( -4.000000000000001776, -27.66249999999999787, 11.30940107675849760 ) ) ;
#12431 =( BOUNDED_CURVE ( )  B_SPLINE_CURVE ( 2, ( #4050, #7602, #19997, #23675, #15831, #21470, #7726, #1969, #5892 ),
 .UNSPECIFIED., .F., .F. ) 
 B_SPLINE_CURVE_WITH_KNOTS ( ( 3, 2, 2, 2, 3 ),
 ( 0.5750000000000000666, 0.5833333333333333703, 0.5999999999999999778, 0.6166666666666666963, 0.6250000000000000000 ),
 .UNSPECIFIED. ) 
 CURVE ( )  GEOMETRIC_REPRESENTATION_ITEM ( )  RATIONAL_B_SPLINE_CURVE ( ( 0.9330127018922194093, 0.9330127018922198534, 1.000000000000000000, 0.8660254037844387076, 1.000000000000000000, 0.8660254037844387076, 1.000000000000000000, 0.9330127018922194093, 0.9330127018922194093 ) ) 
 REPRESENTATION_ITEM ( '' )  );
#12432 = EDGE_LOOP ( 'NONE', ( #17043, #8611, #22469, #15637, #5207, #18205 ) ) ;
#12433 = CARTESIAN_POINT ( 'NONE',  ( 3.469446951953614189E-15, -8.999999999999992895, 0.000000000000000000 ) ) ;
#12434 = CARTESIAN_POINT ( 'NONE',  ( 1.878215178125004048, 25.77812499938548640, 5.746835883940462963 ) ) ;
#12435 = EDGE_CURVE ( 'NONE', #15216, #3025, #14124, .T. ) ;
#12436 = CARTESIAN_POINT ( 'NONE',  ( -3.756430356249995661, -6.831223922626973533, 1.790624999385484806 ) ) ;
#12437 = DIRECTION ( 'NONE',  ( 1.000000000000000000, 0.000000000000000000, -0.000000000000000000 ) ) ;
#12438 = CARTESIAN_POINT ( 'NONE',  ( 21.70609600442870857, 16.39370124850988830, 8.999999999999992895 ) ) ;
#12439 = DIRECTION ( 'NONE',  ( -0.000000000000000000, -0.000000000000000000, -1.000000000000000000 ) ) ;
#12440 = DIRECTION ( 'NONE',  ( 1.000000000000000000, 0.000000000000000000, 0.000000000000000000 ) ) ;
#12441 = CIRCLE ( 'NONE', #25810, 0.5000000000000007772 ) ;
#12442 = CONTEXT_DEPENDENT_SHAPE_REPRESENTATION ( #258, #19060 ) ;
#12443 = CARTESIAN_POINT ( 'NONE',  ( 3.756430356250004099, -6.831223922626973533, 0.6281249993854786107 ) ) ;
#12444 = CARTESIAN_POINT ( 'NONE',  ( -1.999999999999995781, -5.535898384862237620, 4.199999999999999289 ) ) ;
#12445 = CARTESIAN_POINT ( 'NONE',  ( -3.756430356249996105, 28.92812499938548498, 6.831223922626973533 ) ) ;
#12446 = CARTESIAN_POINT ( 'NONE',  ( 3.756430356250003655, -8.999999999999992895, 1.603124999385485028 ) ) ;
#12447 = CARTESIAN_POINT ( 'NONE',  ( -3.959305671612554781E-15, -30.00000000000000355, 12.99999999999999289 ) ) ;
#12448 = CIRCLE ( 'NONE', #3676, 31.10000000000000142 ) ;
#12449 = ORIENTED_EDGE ( 'NONE', *, *, #5292, .T. ) ;
#12450 = ORIENTED_EDGE ( 'NONE', *, *, #16872, .F. ) ;
#12451 = CARTESIAN_POINT ( 'NONE',  ( -1.878215178124998275, 28.25312499938548783, 12.25316411605951927 ) ) ;
#12452 = ORIENTED_EDGE ( 'NONE', *, *, #8826, .F. ) ;
#12453 = DIRECTION ( 'NONE',  ( 0.000000000000000000, 0.000000000000000000, 1.000000000000000000 ) ) ;
#12454 = ORIENTED_EDGE ( 'NONE', *, *, #4105, .T. ) ;
#12455 = CARTESIAN_POINT ( 'NONE',  ( -1.999999999999998224, 28.45000000000000639, 12.46410161513774639 ) ) ;
#12456 = ORIENTED_EDGE ( 'NONE', *, *, #4246, .T. ) ;
#12457 = CARTESIAN_POINT ( 'NONE',  ( 3.999999999999997335, -29.70624999877096784, 11.30940107675849404 ) ) ;
#12458 = CARTESIAN_POINT ( 'NONE',  ( -12.74173596767398742, -28.14012133169310559, 1.000000000000000000 ) ) ;
#12459 = ORIENTED_EDGE ( 'NONE', *, *, #7442, .F. ) ;
#12460 = EDGE_CURVE ( 'NONE', #20546, #7614, #1450, .T. ) ;
#12461 = AXIS2_PLACEMENT_3D ( 'NONE', #18028, #23905, #2442 ) ;
#12462 = DIRECTION ( 'NONE',  ( 0.000000000000000000, 0.000000000000000000, -1.000000000000000000 ) ) ;
#12463 = CARTESIAN_POINT ( 'NONE',  ( -3.756430356249997882, 26.75312499938548427, 11.16877607737301226 ) ) ;
#12464 = LINE ( 'NONE', #16540, #1358 ) ;
#12465 = VECTOR ( 'NONE', #5514, 1000.000000000000000 ) ;
#12466 = DIRECTION ( 'NONE',  ( 0.000000000000000000, -0.000000000000000000, 1.000000000000000000 ) ) ;
#12467 = CARTESIAN_POINT ( 'NONE',  ( -14.48253926456298579, 27.25313774936435962, -6.500000000000000000 ) ) ;
#12468 = EDGE_CURVE ( 'NONE', #17328, #1348, #5119, .T. ) ;
#12469 = CARTESIAN_POINT ( 'NONE',  ( -3.756430356249997882, 28.10312499938548569, 11.16877607737301226 ) ) ;
#12470 = PLANE ( 'NONE',  #16804 ) ;
#12471 = AXIS2_PLACEMENT_3D ( 'NONE', #16707, #4809, #12784 ) ;
#12472 = CIRCLE ( 'NONE', #12858, 31.10000000000000142 ) ;
#12473 = CARTESIAN_POINT ( 'NONE',  ( -0.07793552093707546702, 39.00000000000049027, 3.500000000000446754 ) ) ;
#12474 = CARTESIAN_POINT ( 'NONE',  ( 4.000000000000005329, 25.43124999877097281, 6.690598923241489970 ) ) ;
#12475 = DIRECTION ( 'NONE',  ( 1.000000000000000000, 0.000000000000000000, 0.000000000000000000 ) ) ;
#12477 = CARTESIAN_POINT ( 'NONE',  ( -1.878215178125004048, -25.66562499938548569, 5.746835883940462963 ) ) ;
#12476 = AXIS2_PLACEMENT_3D ( 'NONE', #5291, #1380, #22954 ) ;
#12478 = LINE ( 'NONE', #22172, #7078 ) ;
#12479 = AXIS2_PLACEMENT_3D ( 'NONE', #3908, #7821, #16073 ) ;
#12480 = EDGE_LOOP ( 'NONE', ( #927, #21185, #15465, #9827 ) ) ;
#12481 = CARTESIAN_POINT ( 'NONE',  ( 1.878215178125004048, 25.77812499938548640, 5.746835883940462963 ) ) ;
#12482 = EDGE_CURVE ( 'NONE', #18610, #19636, #11770, .T. ) ;
#12483 = CARTESIAN_POINT ( 'NONE',  ( 1.999999999999998224, -28.44999999999999929, 12.46410161513774639 ) ) ;
#12485 = VERTEX_POINT ( 'NONE', #20518 ) ;
#12484 = CARTESIAN_POINT ( 'NONE',  ( -1.878215178124999829, 28.70312499938548711, 12.25316411605951927 ) ) ;
#12486 = EDGE_LOOP ( 'NONE', ( #20937, #20427, #18970, #20672 ) ) ;
#12487 = DIRECTION ( 'NONE',  ( 1.224646799147353207E-16, 1.000000000000000000, -0.000000000000000000 ) ) ;
#12488 = DIRECTION ( 'NONE',  ( 0.000000000000000000, 0.000000000000000000, -1.000000000000000000 ) ) ;
#12489 = LINE ( 'NONE', #2562, #22999 ) ;
#12490 = EDGE_LOOP ( 'NONE', ( #25, #24209, #6665, #17244 ) ) ;
#12491 = VERTEX_POINT ( 'NONE', #4950 ) ;
#12492 = CARTESIAN_POINT ( 'NONE',  ( -3.756430356250003655, -25.70312499938548356, 8.999999999999992895 ) ) ;
#12493 = CARTESIAN_POINT ( 'NONE',  ( 1.878215178125003382, 27.46562499938548996, 5.746835883940462963 ) ) ;
#12494 = LINE ( 'NONE', #2314, #8037 ) ;
#12495 = EDGE_CURVE ( 'NONE', #20454, #3228, #2613, .T. ) ;
#12496 = CIRCLE ( 'NONE', #6654, 4.000000000000000000 ) ;
#12497 = DIRECTION ( 'NONE',  ( 0.000000000000000000, 0.000000000000000000, 1.000000000000000000 ) ) ;
#12498 = EDGE_CURVE ( 'NONE', #23985, #3679, #20550, .T. ) ;
#12499 = AXIS2_PLACEMENT_3D ( 'NONE', #2538, #22157, #14327 ) ;
#12500 = AXIS2_PLACEMENT_3D ( 'NONE', #24783, #13401, #25176 ) ;
#12501 = CYLINDRICAL_SURFACE ( 'NONE', #7934, 4.000000000000000000 ) ;
#12502 = CARTESIAN_POINT ( 'NONE',  ( 0.000000000000000000, 0.000000000000000000, 0.000000000000000000 ) ) ;
#12503 = EDGE_CURVE ( 'NONE', #24856, #25109, #8551, .T. ) ;
#12504 = DIRECTION ( 'NONE',  ( 1.000000000000000000, 0.000000000000000000, 0.000000000000000000 ) ) ;
#12505 = LINE ( 'NONE', #20620, #7999 ) ;
#12506 = DIRECTION ( 'NONE',  ( 0.000000000000000000, 0.000000000000000000, 1.000000000000000000 ) ) ;
#12507 = CIRCLE ( 'NONE', #15863, 0.5000000000000004441 ) ;
#12508 = CARTESIAN_POINT ( 'NONE',  ( 29.72853858738285737, 9.133673601486366422, -6.500000000000000000 ) ) ;
#12509 = CARTESIAN_POINT ( 'NONE',  ( 21.38789795289476103, 16.07550319697594432, 8.999999999999992895 ) ) ;
#12510 = CARTESIAN_POINT ( 'NONE',  ( 22.37551020630278842, 16.71865595681033412, 8.999999999999992895 ) ) ;
#12511 = CARTESIAN_POINT ( 'NONE',  ( 1.859271017917182139E-15, 28.48749999999999716, 12.99999999999999289 ) ) ;
#12512 = CARTESIAN_POINT ( 'NONE',  ( 18.68225429291714690, -24.86329371854781201, -2.750000000000000000 ) ) ;
#12513 = CARTESIAN_POINT ( 'NONE',  ( 3.735045420075836212E-15, 29.41562499938548569, 4.662447845253954171 ) ) ;
#12515 = VERTEX_POINT ( 'NONE', #653 ) ;
#12514 = CARTESIAN_POINT ( 'NONE',  ( -2.439210544738880326, 29.90146712018378494, 5.819033386899011617 ) ) ;
#12516 = CIRCLE ( 'NONE', #3742, 0.5000000000000017764 ) ;
#12517 = DIRECTION ( 'NONE',  ( 1.000000000000000000, 0.000000000000000000, 0.000000000000000000 ) ) ;
#12518 = CARTESIAN_POINT ( 'NONE',  ( 21.80540536484019043, 16.14855111534773968, 6.690598923241489970 ) ) ;
#12519 = ORIENTED_EDGE ( 'NONE', *, *, #13214, .F. ) ;
#12520 = CARTESIAN_POINT ( 'NONE',  ( -1.999999999999995781, 28.75000000000000000, 5.535898384862237620 ) ) ;
#12521 = CARTESIAN_POINT ( 'NONE',  ( -3.999999999999996003, 25.58124999877097139, 6.690598923241487306 ) ) ;
#12522 = CARTESIAN_POINT ( 'NONE',  ( 3.756430356249996994, -25.36562499938548498, 8.999999999999992895 ) ) ;
#12524 = VERTEX_POINT ( 'NONE', #24561 ) ;
#12523 = CARTESIAN_POINT ( 'NONE',  ( 15.64473753375240506, 21.30159178324472080, 8.999999999999992895 ) ) ;
#12525 = CARTESIAN_POINT ( 'NONE',  ( 3.469446951953614189E-15, 40.00000000000000000, 4.999999999999992006 ) ) ;
#12526 = CIRCLE ( 'NONE', #13379, 0.5000000000000003331 ) ;
#12528 = EDGE_LOOP ( 'NONE', ( #3585, #9023, #24203, #17337, #8581, #24344, #9411, #20154, #14148, #17552, #10645, #19550, #8253, #13748, #25029, #3944, #17424, #23243, #22075, #11987, #14527, #11716, #7415, #18315, #13751 ) ) ;
#12527 = VECTOR ( 'NONE', #10876, 1000.000000000000000 ) ;
#12529 = CARTESIAN_POINT ( 'NONE',  ( 3.756430356249995661, -25.77812499938548640, 6.831223922626973533 ) ) ;
#12530 = ORIENTED_EDGE ( 'NONE', *, *, #10475, .F. ) ;
#12531 = EDGE_LOOP ( 'NONE', ( #5678, #9075, #17390, #18523 ) ) ;
#12532 = DIRECTION ( 'NONE',  ( 0.000000000000000000, -0.000000000000000000, 1.000000000000000000 ) ) ;
#12533 = CARTESIAN_POINT ( 'NONE',  ( 25.45105997952925136, 17.87326343783933780, -6.500000000000000000 ) ) ;
#12534 = CIRCLE ( 'NONE', #15883, 0.5000000000000001110 ) ;
#12535 = PRODUCT_RELATED_PRODUCT_CATEGORY ( 'part', '', ( #7169 ) ) ;
#12536 = CARTESIAN_POINT ( 'NONE',  ( -3.063240906311874401, -29.84319947910909931, 11.57226653943513028 ) ) ;
#12537 = CIRCLE ( 'NONE', #17980, 31.10000000000000142 ) ;
#12538 = AXIS2_PLACEMENT_3D ( 'NONE', #25446, #21790, #7668 ) ;
#12539 = CARTESIAN_POINT ( 'NONE',  ( 1.878215178125004048, -5.746835883940462963, 1.678124999385483651 ) ) ;
#12540 = ADVANCED_FACE ( 'NONE', ( #22620 ), #18683, .T. ) ;
#12541 = CARTESIAN_POINT ( 'NONE',  ( 22.93879470346832150, 19.24746537414215908, 12.11182326528050623 ) ) ;
#12542 = CARTESIAN_POINT ( 'NONE',  ( 1.878215178125004048, 25.21562499938548285, 5.746835883940462963 ) ) ;
#12543 = EDGE_CURVE ( 'NONE', #9673, #6572, #771, .T. ) ;
#12544 = CARTESIAN_POINT ( 'NONE',  ( 2.000000000000003997, -5.535898384862238508, 3.675000000000001155 ) ) ;
#12545 = CARTESIAN_POINT ( 'NONE',  ( 3.735045420075836212E-15, 26.60312499938547859, 4.662447845253954171 ) ) ;
#12546 = CARTESIAN_POINT ( 'NONE',  ( 16.85123847828290167, 22.50809272777520675, 6.690598923241487306 ) ) ;
#12547 = DIRECTION ( 'NONE',  ( 0.000000000000000000, 0.000000000000000000, 1.000000000000000000 ) ) ;
#12548 = CARTESIAN_POINT ( 'NONE',  ( 17.33175248197874652, 18.84750200983072332, 4.999999999999991118 ) ) ;
#12549 = CARTESIAN_POINT ( 'NONE',  ( 3.756430356249996994, -26.37812499938548783, 8.999999999999992895 ) ) ;
#12550 = LINE ( 'NONE', #14272, #25700 ) ;
#12551 = CARTESIAN_POINT ( 'NONE',  ( -12.74173596767339767, 28.14012133169338270, -6.500000000000000000 ) ) ;
#12552 = DIRECTION ( 'NONE',  ( -0.8090169943749417891, 0.5877852522924807976, 0.000000000000000000 ) ) ;
#12553 = CARTESIAN_POINT ( 'NONE',  ( 3.013274039476890653, -29.84885987243285399, 6.356496494711869616 ) ) ;
#12554 = ORIENTED_EDGE ( 'NONE', *, *, #4797, .F. ) ;
#12555 = DIRECTION ( 'NONE',  ( -0.000000000000000000, -1.000000000000000000, -0.000000000000000000 ) ) ;
#12557 = ORIENTED_EDGE ( 'NONE', *, *, #10251, .F. ) ;
#12556 = DIRECTION ( 'NONE',  ( 1.000000000000000000, -2.891205793294678326E-16, 0.000000000000000000 ) ) ;
#12558 = VECTOR ( 'NONE', #915, 1000.000000000000000 ) ;
#12559 = AXIS2_PLACEMENT_3D ( 'NONE', #4464, #20407, #12317 ) ;
#12560 = ORIENTED_EDGE ( 'NONE', *, *, #24953, .T. ) ;
#12561 = EDGE_LOOP ( 'NONE', ( #2452, #966, #20642, #6255 ) ) ;
#12562 = ORIENTED_EDGE ( 'NONE', *, *, #7392, .F. ) ;
#12563 = ORIENTED_EDGE ( 'NONE', *, *, #22316, .T. ) ;
#12564 = TOROIDAL_SURFACE ( 'NONE', #14664, 2.000000000000000000, 2.000000000000000000 ) ;
#12565 = EDGE_LOOP ( 'NONE', ( #21356, #24196 ) ) ;
#12566 = DIRECTION ( 'NONE',  ( 0.000000000000000000, -1.000000000000000000, 0.000000000000000000 ) ) ;
#12567 = AXIS2_PLACEMENT_3D ( 'NONE', #24056, #17914, #11897 ) ;
#12568 = ORIENTED_EDGE ( 'NONE', *, *, #3606, .F. ) ;
#12569 = FACE_OUTER_BOUND ( 'NONE', #2219, .T. ) ;
#12570 = CARTESIAN_POINT ( 'NONE',  ( -3.756430356249996105, 28.14062499938548356, 6.831223922626973533 ) ) ;
#12571 = EDGE_CURVE ( 'NONE', #21735, #20241, #16734, .T. ) ;
#12572 = CARTESIAN_POINT ( 'NONE',  ( 3.735045420075836212E-15, -4.662447845253954171, 3.065624999385482052 ) ) ;
#12573 = PRODUCT_DEFINITION_SHAPE ( 'NONE', 'NONE',  #25878 ) ;
#12574 = CARTESIAN_POINT ( 'NONE',  ( 17.93393197184562027, 20.59012934980492560, 12.25316411605951927 ) ) ;
#12575 = AXIS2_PLACEMENT_3D ( 'NONE', #7400, #15142, #7664 ) ;
#12576 = CARTESIAN_POINT ( 'NONE',  ( 19.55913884271638281, 21.07488837056833830, 4.999999999999987566 ) ) ;
#12577 = EDGE_CURVE ( 'NONE', #17170, #12491, #2600, .T. ) ;
#12578 = AXIS2_PLACEMENT_3D ( 'NONE', #13195, #5468, #1546 ) ;
#12579 = LINE ( 'NONE', #16775, #8363 ) ;
#12580 = CARTESIAN_POINT ( 'NONE',  ( -3.756430356249995661, -6.831223922626973533, 2.128124999385482052 ) ) ;
#12581 = CARTESIAN_POINT ( 'NONE',  ( -13.24173596767339767, 28.14012133169338270, 1.000000000000000000 ) ) ;
#12582 = CARTESIAN_POINT ( 'NONE',  ( 4.000000000000001776, -11.30940107675849760, 4.462500000000000355 ) ) ;
#12583 = DIRECTION ( 'NONE',  ( 0.000000000000000000, 0.000000000000000000, 1.000000000000000000 ) ) ;
#12584 =( BOUNDED_CURVE ( )  B_SPLINE_CURVE ( 2, ( #21987, #20765, #14496, #18673, #759 ),
 .UNSPECIFIED., .F., .T. ) 
 B_SPLINE_CURVE_WITH_KNOTS ( ( 3, 2, 3 ),
 ( 0.9749999999999999778, 0.9833333333333332815, 1.000000000000000000 ),
 .UNSPECIFIED. ) 
 CURVE ( )  GEOMETRIC_REPRESENTATION_ITEM ( )  RATIONAL_B_SPLINE_CURVE ( ( 0.9330127018922194093, 0.9330127018922194093, 1.000000000000000000, 0.8660254037844387076, 1.000000000000000000 ) ) 
 REPRESENTATION_ITEM ( '' )  );
#12585 = CARTESIAN_POINT ( 'NONE',  ( 0.000000000000000000, 29.78124999877097423, 12.99999999999999289 ) ) ;
#12586 = AXIS2_PLACEMENT_3D ( 'NONE', #16572, #2577, #6615 ) ;
#12587 = CARTESIAN_POINT ( 'NONE',  ( -1.878215178124995832, -5.746835883940462963, 2.203124999385484895 ) ) ;
#12588 = CARTESIAN_POINT ( 'NONE',  ( -6.317933499822993682, 30.45149776762736593, -2.750000000000000000 ) ) ;
#12589 = EDGE_LOOP ( 'NONE', ( #5738, #9034, #4329, #17073 ) ) ;
#12590 = ORIENTED_EDGE ( 'NONE', *, *, #7980, .F. ) ;
#12591 = CARTESIAN_POINT ( 'NONE',  ( -3.756430356250000546, 28.21562499938548640, 11.16877607737301226 ) ) ;
#12592 =( BOUNDED_CURVE ( )  B_SPLINE_CURVE ( 2, ( #14090, #1935, #10277, #5717, #18157, #234, #9779, #24287, #24670 ),
 .UNSPECIFIED., .F., .F. ) 
 B_SPLINE_CURVE_WITH_KNOTS ( ( 3, 2, 2, 2, 3 ),
 ( 0.4750000000000000333, 0.4833333333333333370, 0.5000000000000000000, 0.5166666666666667185, 0.5250000000000000222 ),
 .UNSPECIFIED. ) 
 CURVE ( )  GEOMETRIC_REPRESENTATION_ITEM ( )  RATIONAL_B_SPLINE_CURVE ( ( 0.9330127018922194093, 0.9330127018922196314, 1.000000000000000000, 0.8660254037844387076, 1.000000000000000000, 0.8660254037844387076, 1.000000000000000000, 0.9330127018922194093, 0.9330127018922194093 ) ) 
 REPRESENTATION_ITEM ( '' )  );
#12593 = EDGE_CURVE ( 'NONE', #17199, #21622, #4826, .T. ) ;
#12594 = VECTOR ( 'NONE', #5704, 1000.000000000000000 ) ;
#12595 = ORIENTED_EDGE ( 'NONE', *, *, #25631, .T. ) ;
#12596 = DIRECTION ( 'NONE',  ( 0.000000000000000000, 0.000000000000000000, 1.000000000000000000 ) ) ;
#12597 = ORIENTED_EDGE ( 'NONE', *, *, #24350, .F. ) ;
#12598 = CARTESIAN_POINT ( 'NONE',  ( -1.071796769724485454, 26.21740381056766367, 12.99999999999999467 ) ) ;
#12599 = ORIENTED_EDGE ( 'NONE', *, *, #17756, .T. ) ;
#12600 = CARTESIAN_POINT ( 'NONE',  ( 23.94977458897859890, 18.29292033948614105, 10.45670610619353980 ) ) ;
#12601 = CIRCLE ( 'NONE', #5486, 30.00000000000000355 ) ;
#12602 = AXIS2_PLACEMENT_3D ( 'NONE', #2290, #21774, #22160 ) ;
#12603 = DIRECTION ( 'NONE',  ( -0.5877852522924652545, 0.8090169943749532244, 0.000000000000000000 ) ) ;
#12604 = VERTEX_POINT ( 'NONE', #8502 ) ;
#12605 = CARTESIAN_POINT ( 'NONE',  ( -1.952785157361865753, -31.03863125411923463, -6.500000000000000000 ) ) ;
#12606 = CARTESIAN_POINT ( 'NONE',  ( -3.999999999999996003, 25.18750000000000000, 6.690598923241487306 ) ) ;
#12607 = CARTESIAN_POINT ( 'NONE',  ( 17.64231419060439876, 20.47074131535051933, 5.535898384862237620 ) ) ;
#12608 = CIRCLE ( 'NONE', #6756, 31.10000000000000142 ) ;
#12609 = CARTESIAN_POINT ( 'NONE',  ( 3.469446951953614189E-15, 35.50000000000000711, 4.999999999999992006 ) ) ;
#12610 = CARTESIAN_POINT ( 'NONE',  ( -1.071796769724489895, 26.66740381056767006, 12.99999999999999289 ) ) ;
#12611 = CARTESIAN_POINT ( 'NONE',  ( 15.33304107673014727, 20.64543583264882542, 6.831223922626973533 ) ) ;
#12612 = AXIS2_PLACEMENT_3D ( 'NONE', #16349, #24318, #20743 ) ;
#12613 = CARTESIAN_POINT ( 'NONE',  ( 3.756430356250002323, 28.70312499938548356, 11.16877607737301226 ) ) ;
#12614 = AXIS2_PLACEMENT_3D ( 'NONE', #15025, #13069, #16991 ) ;
#12615 = ADVANCED_FACE ( 'NONE', ( #16484 ), #24446, .T. ) ;
#12616 = AXIS2_PLACEMENT_3D ( 'NONE', #21171, #11099, #16743 ) ;
#12617 = CARTESIAN_POINT ( 'NONE',  ( 16.63462326141533865, 19.29082063937464397, 5.746835883940462963 ) ) ;
#12618 = APPLICATION_CONTEXT ( 'automotive_design' ) ;
#12619 = CARTESIAN_POINT ( 'NONE',  ( 23.07819757097597702, 17.42134332148352627, 6.690598923241489970 ) ) ;
#12620 = CIRCLE ( 'NONE', #11367, 0.5000000000000005551 ) ;
#12621 = CARTESIAN_POINT ( 'NONE',  ( -3.999999999999996447, 25.58124999877097494, 6.690598923241487306 ) ) ;
#12622 = LINE ( 'NONE', #20595, #22107 ) ;
#12623 = AXIS2_PLACEMENT_3D ( 'NONE', #4921, #22450, #10669 ) ;
#12624 = CARTESIAN_POINT ( 'NONE',  ( 3.756430356249996994, -27.61562499938548143, 8.999999999999992895 ) ) ;
#12625 = ADVANCED_FACE ( 'NONE', ( #17632 ), #3237, .F. ) ;
#12626 = CARTESIAN_POINT ( 'NONE',  ( 3.752267015613588906E-15, -4.381197846482986158, 1.462499999999998135 ) ) ;
#12627 = ORIENTED_EDGE ( 'NONE', *, *, #18886, .T. ) ;
#12628 = CARTESIAN_POINT ( 'NONE',  ( 2.620986760973688460E-15, 29.78124999877096712, 13.61880215351699874 ) ) ;
#12629 = CARTESIAN_POINT ( 'NONE',  ( -2.000000000000000888, -29.42500000000000071, 12.46410161513774817 ) ) ;
#12631 = ORIENTED_EDGE ( 'NONE', *, *, #18891, .F. ) ;
#12630 = DIRECTION ( 'NONE',  ( 1.000000000000000000, 0.000000000000000000, 0.000000000000000000 ) ) ;
#12632 = ORIENTED_EDGE ( 'NONE', *, *, #4746, .F. ) ;
#12633 = LINE ( 'NONE', #18645, #2464 ) ;
#12634 = AXIS2_PLACEMENT_3D ( 'NONE', #9420, #15572, #21452 ) ;
#12635 = DIRECTION ( 'NONE',  ( 1.000000000000000000, 0.000000000000000000, 0.000000000000000000 ) ) ;
#12636 = ORIENTED_EDGE ( 'NONE', *, *, #6855, .F. ) ;
#12637 = CARTESIAN_POINT ( 'NONE',  ( -1.878215178125000939, -26.52812499938548285, 12.25316411605952283 ) ) ;
#12638 = CARTESIAN_POINT ( 'NONE',  ( 3.756430356250003211, 28.74062499938548498, 8.999999999999992895 ) ) ;
#12639 = CARTESIAN_POINT ( 'NONE',  ( 2.000000000000003997, 28.16874999877096997, 5.535898384862238508 ) ) ;
#12640 = AXIS2_PLACEMENT_3D ( 'NONE', #20819, #18726, #6695 ) ;
#12641 = CARTESIAN_POINT ( 'NONE',  ( 2.672651547586948120E-15, -13.33755215474603162, 4.528124999385480187 ) ) ;
#12642 = CARTESIAN_POINT ( 'NONE',  ( 3.756430356250002323, 27.42812499938548498, 6.831223922626973533 ) ) ;
#12643 = FACE_OUTER_BOUND ( 'NONE', #2528, .T. ) ;
#12644 = DIRECTION ( 'NONE',  ( 0.7071067811865463515, -0.7071067811865487940, 0.000000000000000000 ) ) ;
#12645 = CARTESIAN_POINT ( 'NONE',  ( -7.734255490826573265, 30.12293631110053838, -6.500000000000000000 ) ) ;
#12646 = DIRECTION ( 'NONE',  ( -0.2588190451025209615, 0.9659258262890682012, 0.000000000000000000 ) ) ;
#12647 = AXIS2_PLACEMENT_3D ( 'NONE', #13063, #23128, #20901 ) ;
#12648 = EDGE_CURVE ( 'NONE', #8071, #18519, #11211, .T. ) ;
#12649 = CYLINDRICAL_SURFACE ( 'NONE', #7991, 31.10000000000000142 ) ;
#12650 = CARTESIAN_POINT ( 'NONE',  ( 20.37793354945079471, 17.54950642470453204, 5.535898384862238508 ) ) ;
#12651 = CARTESIAN_POINT ( 'NONE',  ( 18.33395301051795911, 18.33395301051789161, 13.33755215474602984 ) ) ;
#12652 = CARTESIAN_POINT ( 'NONE',  ( 15.67775563255858984, 20.99015038847727155, 8.999999999999992895 ) ) ;
#12653 = DIRECTION ( 'NONE',  ( 0.000000000000000000, -0.000000000000000000, 1.000000000000000000 ) ) ;
#12654 = CARTESIAN_POINT ( 'NONE',  ( 25.16042852506077665, -18.28012134629603835, -6.500000000000000000 ) ) ;
#12655 = CARTESIAN_POINT ( 'NONE',  ( -3.756430356249995661, 29.04062499938548569, 6.831223922626973533 ) ) ;
#12656 = AXIS2_PLACEMENT_3D ( 'NONE', #7957, #19466, #24036 ) ;
#12659 = EDGE_CURVE ( 'NONE', #2116, #12039, #23135, .T. ) ;
#12658 = EDGE_LOOP ( 'NONE', ( #7864, #16199, #21591, #9029 ) ) ;
#12657 = LINE ( 'NONE', #8991, #14986 ) ;
#12660 = CARTESIAN_POINT ( 'NONE',  ( 19.37037015225818948, 16.71417277429875625, 12.25316411605952283 ) ) ;
#12661 = CARTESIAN_POINT ( 'NONE',  ( 1.999999999999995781, -27.85000000000000142, 5.535898384862237620 ) ) ;
#12662 = VERTEX_POINT ( 'NONE', #25605 ) ;
#12663 = FACE_OUTER_BOUND ( 'NONE', #22952, .T. ) ;
#12664 = CARTESIAN_POINT ( 'NONE',  ( 4.000000000000003553, 28.54374999877096997, 8.999999999999992895 ) ) ;
#12665 = CARTESIAN_POINT ( 'NONE',  ( 3.756430356249996994, -27.61562499938548143, 8.999999999999992895 ) ) ;
#12667 = ORIENTED_EDGE ( 'NONE', *, *, #23305, .F. ) ;
#12666 = FACE_OUTER_BOUND ( 'NONE', #10081, .T. ) ;
#12668 = EDGE_CURVE ( 'NONE', #23953, #23031, #4945, .T. ) ;
#12669 = DIRECTION ( 'NONE',  ( 0.000000000000000000, 0.000000000000000000, 1.000000000000000000 ) ) ;
#12670 = AXIS2_PLACEMENT_3D ( 'NONE', #16420, #22412, #18508 ) ;
#12671 = ORIENTED_EDGE ( 'NONE', *, *, #24526, .T. ) ;
#12672 = CARTESIAN_POINT ( 'NONE',  ( -3.756430356250003655, -26.49062499938548498, 8.999999999999992895 ) ) ;
#12673 = VERTEX_POINT ( 'NONE', #1674 ) ;
#12674 = EDGE_CURVE ( 'NONE', #7614, #4649, #2284, .T. ) ;
#12675 = ORIENTED_EDGE ( 'NONE', *, *, #23124, .F. ) ;
#12676 = CARTESIAN_POINT ( 'NONE',  ( -3.137519842735244810E-15, 26.91249999999999787, 4.999999999999991118 ) ) ;
#12677 = CYLINDRICAL_SURFACE ( 'NONE', #104, 4.000000000000000000 ) ;
#12678 = CARTESIAN_POINT ( 'NONE',  ( 1.626862140677534194E-14, 27.58750000000000213, 12.99999999999999289 ) ) ;
#12679 = CARTESIAN_POINT ( 'NONE',  ( 3.756430356250002323, -11.16877607737301226, 2.465624999385482852 ) ) ;
#12680 = SHAPE_REPRESENTATION_RELATIONSHIP ( 'NONE' , 'NONE' ,  #8162, #1303 ) ;
#12681 = ADVANCED_FACE ( 'NONE', ( #15407 ), #15282, .F. ) ;
#12682 = CARTESIAN_POINT ( 'NONE',  ( -3.041313392017702455, 38.65031218604096352, 4.002974454653567271 ) ) ;
#12683 = CARTESIAN_POINT ( 'NONE',  ( 3.735045420075836212E-15, 28.85312499938548569, 4.662447845253954171 ) ) ;
#12684 = DIRECTION ( 'NONE',  ( 0.000000000000000000, 0.000000000000000000, 1.000000000000000000 ) ) ;
#12685 = CARTESIAN_POINT ( 'NONE',  ( 21.21320343559646915, 21.21320343559638744, 4.999999999999992006 ) ) ;
#12686 = STYLED_ITEM ( 'NONE', ( #9426 ), #14134 ) ;
#12687 = CARTESIAN_POINT ( 'NONE',  ( -3.756430356249996994, 27.61562499938548143, 8.999999999999992895 ) ) ;
#12688 = DIRECTION ( 'NONE',  ( -0.9510565162951518658, 0.3090169943749528914, 0.000000000000000000 ) ) ;
#12689 = CARTESIAN_POINT ( 'NONE',  ( 18.39361514561510091, 18.39361514561503341, 4.999999999999992006 ) ) ;
#12690 = CARTESIAN_POINT ( 'NONE',  ( -3.756430356250002323, -26.11562499938548498, 11.16877607737301226 ) ) ;
#12691 = CARTESIAN_POINT ( 'NONE',  ( 3.756430356250003655, 29.30312499938548498, 8.999999999999992895 ) ) ;
#12692 = CARTESIAN_POINT ( 'NONE',  ( -25.75859848311247902, 16.66421332384710752, 1.000000000000000000 ) ) ;
#12693 = CIRCLE ( 'NONE', #9749, 31.10000000000000142 ) ;
#12694 = CARTESIAN_POINT ( 'NONE',  ( 0.7500000000000001110, 1.299038105676658450, 17.69999999999999929 ) ) ;
#12695 = CARTESIAN_POINT ( 'NONE',  ( 3.796077574538131660, -29.75903253174124430, 10.28786097927510923 ) ) ;
#12696 = ORIENTED_EDGE ( 'NONE', *, *, #6858, .F. ) ;
#12697 = DIRECTION ( 'NONE',  ( -0.000000000000000000, -0.000000000000000000, -1.000000000000000000 ) ) ;
#12699 = VERTEX_POINT ( 'NONE', #13696 ) ;
#12698 = CARTESIAN_POINT ( 'NONE',  ( 3.752267015613588906E-15, -4.381197846482986158, 3.656249998770967569 ) ) ;
#12700 = EDGE_CURVE ( 'NONE', #2753, #25495, #23249, .T. ) ;
#12701 = ORIENTED_EDGE ( 'NONE', *, *, #1688, .F. ) ;
#12702 = VERTEX_POINT ( 'NONE', #15545 ) ;
#12703 = ORIENTED_EDGE ( 'NONE', *, *, #9244, .T. ) ;
#12704 = EDGE_CURVE ( 'NONE', #14144, #22219, #20127, .T. ) ;
#12705 = ORIENTED_EDGE ( 'NONE', *, *, #2692, .F. ) ;
#12706 = LINE ( 'NONE', #14529, #8023 ) ;
#12707 = ADVANCED_FACE ( 'NONE', ( #7557 ), #3507, .F. ) ;
#12708 =( BOUNDED_CURVE ( )  B_SPLINE_CURVE ( 2, ( #5359, #25366, #23159, #10500, #3401, #22538, #13219, #23408, #3263 ),
 .UNSPECIFIED., .F., .F. ) 
 B_SPLINE_CURVE_WITH_KNOTS ( ( 3, 2, 2, 2, 3 ),
 ( 0.8250000000000000666, 0.8333333333333333703, 0.8499999999999999778, 0.8666666666666666963, 0.8750000000000000000 ),
 .UNSPECIFIED. ) 
 CURVE ( )  GEOMETRIC_REPRESENTATION_ITEM ( )  RATIONAL_B_SPLINE_CURVE ( ( 0.9330127018922194093, 0.9330127018922198534, 1.000000000000000000, 0.8660254037844387076, 1.000000000000000000, 0.8660254037844387076, 1.000000000000000000, 0.9330127018922194093, 0.9330127018922194093 ) ) 
 REPRESENTATION_ITEM ( '' )  );
#12709 = STYLED_ITEM ( 'NONE', ( #22967 ), #13495 ) ;
#12710 = ORIENTED_EDGE ( 'NONE', *, *, #5202, .F. ) ;
#12711 = DIRECTION ( 'NONE',  ( 0.000000000000000000, 0.000000000000000000, -1.000000000000000000 ) ) ;
#12712 = CARTESIAN_POINT ( 'NONE',  ( 1.878215178125004048, 28.02812499938548640, 5.746835883940462963 ) ) ;
#12713 = CARTESIAN_POINT ( 'NONE',  ( 3.735045420075836212E-15, -4.662447845253954171, 1.715624999385482852 ) ) ;
#12714 = DIRECTION ( 'NONE',  ( 0.000000000000000000, 0.000000000000000000, -1.000000000000000000 ) ) ;
#12715 = CARTESIAN_POINT ( 'NONE',  ( 20.24314131972164432, 20.24314131972156972, 13.33755215474602984 ) ) ;
#12716 = FACE_OUTER_BOUND ( 'NONE', #15275, .T. ) ;
#12717 = CARTESIAN_POINT ( 'NONE',  ( -13.02991752792603997, -22.56362157461194684, 20.00001200000000168 ) ) ;
#12718 = CARTESIAN_POINT ( 'NONE',  ( 3.735045420075836212E-15, -4.662447845253954171, 2.953124999385479565 ) ) ;
#12719 = CARTESIAN_POINT ( 'NONE',  ( -30.85476721088022600, 3.897863563850190616, -6.500000000000000000 ) ) ;
#12720 = CARTESIAN_POINT ( 'NONE',  ( 4.000000000000003553, -6.690598923241489970, 3.637499999999998845 ) ) ;
#12721 = CARTESIAN_POINT ( 'NONE',  ( 0.000000000000000000, 0.000000000000000000, -6.500000000000000000 ) ) ;
#12722 = DIRECTION ( 'NONE',  ( -0.5358267949789882190, 0.8443279255020205154, 0.000000000000000000 ) ) ;
#12723 = CARTESIAN_POINT ( 'NONE',  ( -3.756430356249997438, -11.16877607737301048, 2.315624999385482496 ) ) ;
#12724 = DIRECTION ( 'NONE',  ( -0.000000000000000000, -0.000000000000000000, -1.000000000000000000 ) ) ;
#12725 = CARTESIAN_POINT ( 'NONE',  ( -25.16042852506064165, 18.28012134629622309, 1.000000000000000000 ) ) ;
#12726 = VERTEX_POINT ( 'NONE', #19452 ) ;
#12727 = EDGE_LOOP ( 'NONE', ( #11407, #23431 ) ) ;
#12728 = CARTESIAN_POINT ( 'NONE',  ( -3.756430356249998326, 29.04062499938548569, 6.831223922626973533 ) ) ;
#12729 = EDGE_LOOP ( 'NONE', ( #16531, #14501, #8941, #22859 ) ) ;
#12730 = FACE_OUTER_BOUND ( 'NONE', #17486, .T. ) ;
#12731 = ORIENTED_EDGE ( 'NONE', *, *, #18466, .F. ) ;
#12732 = CARTESIAN_POINT ( 'NONE',  ( 3.756430356249996994, -25.92812499938548498, 8.999999999999992895 ) ) ;
#12733 = EDGE_CURVE ( 'NONE', #20576, #24829, #14313, .T. ) ;
#12734 = ORIENTED_EDGE ( 'NONE', *, *, #14533, .F. ) ;
#12735 = CARTESIAN_POINT ( 'NONE',  ( -0.5000000000000000000, 0.000000000000000000, 20.00000000000000000 ) ) ;
#12736 = ADVANCED_FACE ( 'NONE', ( #5600 ), #19069, .F. ) ;
#12737 = VERTEX_POINT ( 'NONE', #25092 ) ;
#12738 = CARTESIAN_POINT ( 'NONE',  ( -31.06601413805604039, -1.453535542772269595, -6.500000000000000000 ) ) ;
#12739 = CARTESIAN_POINT ( 'NONE',  ( 4.000000000000003553, 25.93750000000000000, 6.690598923241489970 ) ) ;
#12740 = EDGE_CURVE ( 'NONE', #17935, #12275, #5123, .T. ) ;
#12741 = CARTESIAN_POINT ( 'NONE',  ( -28.34936733434187062, 12.78762572734086866, 1.000000000000000000 ) ) ;
#12742 = DIRECTION ( 'NONE',  ( 0.000000000000000000, 0.000000000000000000, -1.000000000000000000 ) ) ;
#12743 = DIRECTION ( 'NONE',  ( -0.000000000000000000, -1.000000000000000000, -0.000000000000000000 ) ) ;
#12744 = CARTESIAN_POINT ( 'NONE',  ( 19.87418373385361292, 17.21798635589416548, 5.746835883940462963 ) ) ;
#12745 = CARTESIAN_POINT ( 'NONE',  ( -3.756430356249995661, 28.92812499938548143, 6.831223922626973533 ) ) ;
#12746 =( BOUNDED_CURVE ( )  B_SPLINE_CURVE ( 2, ( #10699, #10969, #20655, #18954, #4830, #24449, #6527, #12806, #8625 ),
 .UNSPECIFIED., .F., .F. ) 
 B_SPLINE_CURVE_WITH_KNOTS ( ( 3, 2, 2, 2, 3 ),
 ( 0.8250000000000000666, 0.8333333333333333703, 0.8499999999999999778, 0.8666666666666666963, 0.8750000000000000000 ),
 .UNSPECIFIED. ) 
 CURVE ( )  GEOMETRIC_REPRESENTATION_ITEM ( )  RATIONAL_B_SPLINE_CURVE ( ( 0.9330127018922194093, 0.9330127018922198534, 1.000000000000000000, 0.8660254037844387076, 1.000000000000000000, 0.8660254037844387076, 1.000000000000000000, 0.9330127018922194093, 0.9330127018922194093 ) ) 
 REPRESENTATION_ITEM ( '' )  );
#12747 = CARTESIAN_POINT ( 'NONE',  ( 3.469446951953614189E-15, 31.50000000000000000, 8.999999999999992895 ) ) ;
#12748 = FACE_OUTER_BOUND ( 'NONE', #23661, .T. ) ;
#12749 = ORIENTED_EDGE ( 'NONE', *, *, #4067, .T. ) ;
#12750 = CARTESIAN_POINT ( 'NONE',  ( 3.469446951953614189E-15, -8.999999999999992895, 25.00000000000000000 ) ) ;
#12751 = CARTESIAN_POINT ( 'NONE',  ( -23.96296185032722548, -19.82388608118403539, 1.000000000000000000 ) ) ;
#12752 = DIRECTION ( 'NONE',  ( 1.000000000000000000, 0.000000000000000000, 0.000000000000000000 ) ) ;
#12753 = CARTESIAN_POINT ( 'NONE',  ( 3.756430356249996994, -28.06562499938548427, 8.999999999999992895 ) ) ;
#12754 = AXIS2_PLACEMENT_3D ( 'NONE', #24715, #10196, #276 ) ;
#12755 = CARTESIAN_POINT ( 'NONE',  ( 4.000000000000003553, -8.999999999999992895, 1.350000000000000533 ) ) ;
#12756 = CARTESIAN_POINT ( 'NONE',  ( 3.756430356250002323, 26.56562499938548427, 11.16877607737301226 ) ) ;
#12757 = CARTESIAN_POINT ( 'NONE',  ( 2.875168806925156861, 29.86250404960532379, 11.79623638833883525 ) ) ;
#12759 = ORIENTED_EDGE ( 'NONE', *, *, #2922, .T. ) ;
#12758 = CARTESIAN_POINT ( 'NONE',  ( -3.756430356249994773, 29.07812499938548711, 8.999999999999992895 ) ) ;
#12760 = ADVANCED_FACE ( 'NONE', ( #6104 ), #7940, .T. ) ;
#12761 = EDGE_LOOP ( 'NONE', ( #6546, #5446, #9256 ) ) ;
#12762 = DIRECTION ( 'NONE',  ( 0.000000000000000000, 0.000000000000000000, 1.000000000000000000 ) ) ;
#12763 = EDGE_CURVE ( 'NONE', #7410, #11752, #4272, .T. ) ;
#12764 = CARTESIAN_POINT ( 'NONE',  ( 2.000000000000000888, -12.46410161513774817, 4.368749998770966592 ) ) ;
#12765 = ORIENTED_EDGE ( 'NONE', *, *, #3935, .T. ) ;
#12766 = CARTESIAN_POINT ( 'NONE',  ( 3.756430356249996105, -26.34062499938548285, 6.831223922626973533 ) ) ;
#12767 = CARTESIAN_POINT ( 'NONE',  ( 4.000000000000001776, 25.86250000000000071, 11.30940107675849760 ) ) ;
#12768 = CARTESIAN_POINT ( 'NONE',  ( 1.878215178125006934, 26.56562499938548783, 5.746835883940462963 ) ) ;
#12769 = CIRCLE ( 'NONE', #678, 0.5000000000000009992 ) ;
#12770 = CARTESIAN_POINT ( 'NONE',  ( 0.000000000000000000, 0.000000000000000000, -6.500000000000000000 ) ) ;
#12771 = CARTESIAN_POINT ( 'NONE',  ( 4.006172263299091013E-15, 25.33750000000000924, 13.61880215351699874 ) ) ;
#12772 = EDGE_CURVE ( 'NONE', #18967, #10560, #21810, .T. ) ;
#12773 = CARTESIAN_POINT ( 'NONE',  ( 4.648177544792955347E-16, 28.93750000000000355, 12.99999999999999289 ) ) ;
#12774 = CARTESIAN_POINT ( 'NONE',  ( -1.999999999999995781, -5.535898384862237620, 1.049999999999998934 ) ) ;
#12775 = VECTOR ( 'NONE', #18286, 1000.000000000000000 ) ;
#12776 = CARTESIAN_POINT ( 'NONE',  ( -16.66421332384701515, -26.25859848311253941, -6.500000000000000000 ) ) ;
#12777 = CARTESIAN_POINT ( 'NONE',  ( 26.49999999999999645, 0.5000000000000000000, 19.50000000000000000 ) ) ;
#12778 = CARTESIAN_POINT ( 'NONE',  ( -15.41874213889376044, 27.00874656207322388, -2.750000000000000000 ) ) ;
#12779 = CARTESIAN_POINT ( 'NONE',  ( 19.60674521665374215, 19.60674521665367820, 13.33755215474602984 ) ) ;
#12780 = CARTESIAN_POINT ( 'NONE',  ( 18.15054718871317974, 23.80740143820548482, 8.999999999999992895 ) ) ;
#12781 = CARTESIAN_POINT ( 'NONE',  ( -23.64116323484252291, -20.20656826142258211, -2.750000000000000000 ) ) ;
#12782 = DIRECTION ( 'NONE',  ( 0.000000000000000000, 0.000000000000000000, 1.000000000000000000 ) ) ;
#12783 = CARTESIAN_POINT ( 'NONE',  ( -1.878215178124995832, 27.54062499938548214, 5.746835883940462963 ) ) ;
#12784 = DIRECTION ( 'NONE',  ( 1.000000000000000000, 0.000000000000000000, 0.000000000000000000 ) ) ;
#12785 = CARTESIAN_POINT ( 'NONE',  ( -1.859271017917182139E-15, -28.48749999999999716, 12.99999999999999289 ) ) ;
#12786 = CARTESIAN_POINT ( 'NONE',  ( 19.78573162020706988, 19.78573162020698462, 12.99999999999999289 ) ) ;
#12787 = AXIS2_PLACEMENT_3D ( 'NONE', #7587, #10053, #1841 ) ;
#12788 = ORIENTED_EDGE ( 'NONE', *, *, #17860, .T. ) ;
#12789 = CARTESIAN_POINT ( 'NONE',  ( -1.999999999999998224, 28.39374999877096784, 12.46410161513774639 ) ) ;
#12790 = CARTESIAN_POINT ( 'NONE',  ( 3.756430356249995661, -26.22812499938548214, 6.831223922626973533 ) ) ;
#12792 = ORIENTED_EDGE ( 'NONE', *, *, #5762, .F. ) ;
#12791 = CARTESIAN_POINT ( 'NONE',  ( -3.999999999999995559, 25.58124999877096784, 6.690598923241487306 ) ) ;
#12793 = LINE ( 'NONE', #12525, #9981 ) ;
#12794 = VERTEX_POINT ( 'NONE', #10274 ) ;
#12795 = CARTESIAN_POINT ( 'NONE',  ( -3.735045420075836212E-15, -26.60312499938547859, 4.662447845253954171 ) ) ;
#12796 = ORIENTED_EDGE ( 'NONE', *, *, #2432, .F. ) ;
#12797 = EDGE_LOOP ( 'NONE', ( #15084, #3143, #6313, #7708 ) ) ;
#12798 =( LENGTH_UNIT ( ) NAMED_UNIT ( * ) SI_UNIT ( .MILLI., .METRE. ) );
#12799 = CARTESIAN_POINT ( 'NONE',  ( 1.878215178125001605, 27.87812499938548783, 12.25316411605952283 ) ) ;
#12800 = EDGE_CURVE ( 'NONE', #3609, #4893, #15788, .T. ) ;
#12801 = CARTESIAN_POINT ( 'NONE',  ( 4.000000000000003553, -8.999999999999992895, 1.799999999999999600 ) ) ;
#12802 = CARTESIAN_POINT ( 'NONE',  ( 3.756430356250003655, -8.999999999999992895, 2.053124999385484095 ) ) ;
#12803 = CARTESIAN_POINT ( 'NONE',  ( -4.000000000000003553, -27.19374999877096855, 8.999999999999992895 ) ) ;
#12804 = CARTESIAN_POINT ( 'NONE',  ( 1.878215178125004048, 28.36562499938548143, 5.746835883940462963 ) ) ;
#12805 = CARTESIAN_POINT ( 'NONE',  ( 30.78811501957143548, -4.393401135981102712, 1.000000000000000000 ) ) ;
#12806 = CARTESIAN_POINT ( 'NONE',  ( 1.071796769724488563, -28.91740381056766651, 12.99999999999999289 ) ) ;
#12807 = UNCERTAINTY_MEASURE_WITH_UNIT (LENGTH_MEASURE( 1.000000000000000082E-05 ), #8621, 'distance_accuracy_value', 'NONE');
#12808 = UNCERTAINTY_MEASURE_WITH_UNIT (LENGTH_MEASURE( 1.000000000000000082E-05 ), #3892, 'distance_accuracy_value', 'NONE');
#12809 = CARTESIAN_POINT ( 'NONE',  ( -4.393401135980685268, 30.78811501957149588, 1.000000000000000000 ) ) ;
#12810 = CYLINDRICAL_SURFACE ( 'NONE', #5039, 4.000000000000000000 ) ;
#12811 = CARTESIAN_POINT ( 'NONE',  ( 21.41845328966172346, 21.00795358153114378, 12.99999999999999112 ) ) ;
#12812 = CARTESIAN_POINT ( 'NONE',  ( 3.469446951953614189E-15, 34.00000000000000000, 8.999999999999992895 ) ) ;
#12813 = CARTESIAN_POINT ( 'NONE',  ( 1.878215178124995832, -26.75312499938548783, 5.746835883940462963 ) ) ;
#12814 = CARTESIAN_POINT ( 'NONE',  ( 1.878215178125000939, 25.62812499938548783, 12.25316411605952283 ) ) ;
#12815 = CARTESIAN_POINT ( 'NONE',  ( 20.92219106202050583, 23.01025686871638598, -6.500000000000000000 ) ) ;
#12816 = DIRECTION ( 'NONE',  ( 0.000000000000000000, 0.000000000000000000, 1.000000000000000000 ) ) ;
#12817 = CARTESIAN_POINT ( 'NONE',  ( 2.439210544738880326, -29.90146712018378494, 5.819033386899011617 ) ) ;
#12818 = VERTEX_POINT ( 'NONE', #3894 ) ;
#12819 = CARTESIAN_POINT ( 'NONE',  ( -30.54913349766228592, -5.827558883615738594, -6.500000000000000000 ) ) ;
#12821 = EDGE_LOOP ( 'NONE', ( #23891, #9704 ) ) ;
#12820 = CARTESIAN_POINT ( 'NONE',  ( 16.66421332384664566, -26.25859848311276679, -6.500000000000000000 ) ) ;
#12822 = EDGE_LOOP ( 'NONE', ( #12824, #12869, #6538, #25630 ) ) ;
#12823 = VERTEX_POINT ( 'NONE', #22194 ) ;
#12824 = ORIENTED_EDGE ( 'NONE', *, *, #2700, .F. ) ;
#12825 = EDGE_CURVE ( 'NONE', #22434, #20048, #21935, .T. ) ;
#12826 = EDGE_LOOP ( 'NONE', ( #7767, #2213, #1235, #3145 ) ) ;
#12827 = CYLINDRICAL_SURFACE ( 'NONE', #23075, 4.000000000000000000 ) ;
#12828 = ORIENTED_EDGE ( 'NONE', *, *, #1570, .F. ) ;
#12829 = DIRECTION ( 'NONE',  ( 1.000000000000000000, 0.000000000000000000, 0.000000000000000000 ) ) ;
#12830 = CARTESIAN_POINT ( 'NONE',  ( -3.756430356249996994, 29.52812499938548640, 8.999999999999992895 ) ) ;
#12831 = EDGE_CURVE ( 'NONE', #25296, #12101, #16176, .T. ) ;
#12832 = CARTESIAN_POINT ( 'NONE',  ( 3.756430356250002323, -11.16877607737301226, 4.715624999385485516 ) ) ;
#12833 = CARTESIAN_POINT ( 'NONE',  ( 1.071796769724492338, 29.40759618943233278, 12.99999999999999467 ) ) ;
#12834 = EDGE_CURVE ( 'NONE', #7795, #13776, #13966, .T. ) ;
#12835 = CARTESIAN_POINT ( 'NONE',  ( 3.735045420075836212E-15, 25.36562499938548498, 4.662447845253954171 ) ) ;
#12836 = CARTESIAN_POINT ( 'NONE',  ( 19.58805710660147170, -17.18149551509900519, 20.00001200000000523 ) ) ;
#12837 = CARTESIAN_POINT ( 'NONE',  ( 1.878215178125000939, -12.25316411605952283, 4.115624999385482319 ) ) ;
#12838 = CARTESIAN_POINT ( 'NONE',  ( -26.25859848311282363, -16.66421332384654974, 1.000000000000000000 ) ) ;
#12840 = EDGE_CURVE ( 'NONE', #19322, #3259, #13055, .T. ) ;
#12839 = DIRECTION ( 'NONE',  ( 0.8090169943749532244, 0.5877852522924652545, 0.000000000000000000 ) ) ;
#12841 = CARTESIAN_POINT ( 'NONE',  ( -12.78762572734076919, -28.34936733434192035, 1.000000000000000000 ) ) ;
#12842 = DIRECTION ( 'NONE',  ( 0.000000000000000000, -1.000000000000000000, 0.000000000000000000 ) ) ;
#12843 = CARTESIAN_POINT ( 'NONE',  ( -1.878215178124998497, -12.25316411605951927, 1.903124999385483296 ) ) ;
#12844 = CARTESIAN_POINT ( 'NONE',  ( 31.03863125411925239, 1.952785157361540236, 1.000000000000000000 ) ) ;
#12845 = CARTESIAN_POINT ( 'NONE',  ( -29.62293631110050995, -7.734255490826679846, -6.500000000000000000 ) ) ;
#12846 = ORIENTED_EDGE ( 'NONE', *, *, #6052, .F. ) ;
#12847 = VERTEX_POINT ( 'NONE', #11980 ) ;
#12848 = DIRECTION ( 'NONE',  ( 0.000000000000000000, -0.000000000000000000, 1.000000000000000000 ) ) ;
#12849 = ORIENTED_EDGE ( 'NONE', *, *, #8035, .T. ) ;
#12850 = DIRECTION ( 'NONE',  ( -0.000000000000000000, 0.000000000000000000, 1.000000000000000000 ) ) ;
#12851 = ORIENTED_EDGE ( 'NONE', *, *, #2692, .T. ) ;
#12852 = CARTESIAN_POINT ( 'NONE',  ( -1.878215178125004048, -26.22812499938548569, 5.746835883940462963 ) ) ;
#12853 = ORIENTED_EDGE ( 'NONE', *, *, #24055, .T. ) ;
#12854 = FACE_OUTER_BOUND ( 'NONE', #11658, .T. ) ;
#12855 = VERTEX_POINT ( 'NONE', #19953 ) ;
#12856 = CARTESIAN_POINT ( 'NONE',  ( -1.999999999999998224, 25.30000000000000426, 12.46410161513774639 ) ) ;
#12857 = CARTESIAN_POINT ( 'NONE',  ( -1.071796769724481901, 28.41115380933862866, 12.99999999999999645 ) ) ;
#12858 = AXIS2_PLACEMENT_3D ( 'NONE', #13007, #3311, #7250 ) ;
#12859 = CARTESIAN_POINT ( 'NONE',  ( 3.469446951953614189E-15, -8.999999999999992895, -10.00000000000000000 ) ) ;
#12860 = CARTESIAN_POINT ( 'NONE',  ( -3.999999999999996447, 28.31874999877096855, 8.999999999999992895 ) ) ;
#12861 = CARTESIAN_POINT ( 'NONE',  ( 16.02247018838703241, 21.33486494430570701, 11.16877607737301226 ) ) ;
#12862 = CARTESIAN_POINT ( 'NONE',  ( -3.999999999999996447, 28.37500000000000000, 8.999999999999992895 ) ) ;
#12863 = VECTOR ( 'NONE', #4716, 1000.000000000000000 ) ;
#12864 = EDGE_CURVE ( 'NONE', #19636, #18810, #16313, .T. ) ;
#12865 = CARTESIAN_POINT ( 'NONE',  ( -3.756430356249995661, 27.12812499938548427, 6.831223922626973533 ) ) ;
#12866 = EDGE_CURVE ( 'NONE', #7097, #13890, #419, .T. ) ;
#12867 = CARTESIAN_POINT ( 'NONE',  ( 22.10384356884614121, 16.79144881292732450, 8.999999999999992895 ) ) ;
#12868 = CARTESIAN_POINT ( 'NONE',  ( 29.41953157733091118, -10.08469938919497721, 1.000000000000000000 ) ) ;
#12869 = ORIENTED_EDGE ( 'NONE', *, *, #19981, .T. ) ;
#12870 = CARTESIAN_POINT ( 'NONE',  ( -23.01025686871616216, 20.92219106202074741, 1.000000000000000000 ) ) ;
#12871 = CARTESIAN_POINT ( 'NONE',  ( -1.999999999999996669, 26.59374999877097423, 12.46410161513774639 ) ) ;
#12872 = EDGE_CURVE ( 'NONE', #6382, #10805, #4279, .T. ) ;
#12873 = CARTESIAN_POINT ( 'NONE',  ( -3.735045420075836212E-15, -28.40312499938548640, 4.662447845253954171 ) ) ;
#12874 = AXIS2_PLACEMENT_3D ( 'NONE', #13234, #19371, #18993 ) ;
#12875 = DIRECTION ( 'NONE',  ( -0.000000000000000000, -0.000000000000000000, 1.000000000000000000 ) ) ;
#12876 = CARTESIAN_POINT ( 'NONE',  ( -1.878215178124995832, 25.85312499938548569, 5.746835883940462963 ) ) ;
#12878 = ORIENTED_EDGE ( 'NONE', *, *, #19831, .T. ) ;
#12877 = CARTESIAN_POINT ( 'NONE',  ( 2.672651547586948120E-15, -13.33755215474602984, 0.4781249993854826963 ) ) ;
#12879 = ORIENTED_EDGE ( 'NONE', *, *, #11092, .T. ) ;
#12880 = CARTESIAN_POINT ( 'NONE',  ( -1.499999999999998224, -10.49999999999999289, 25.00000000000000000 ) ) ;
#12881 = ADVANCED_FACE ( 'NONE', ( #9777, #8080 ), #16058, .T. ) ;
#12882 = CARTESIAN_POINT ( 'NONE',  ( 0.000000000000000000, 0.000000000000000000, -6.500000000000000000 ) ) ;
#12883 = VECTOR ( 'NONE', #24117, 1000.000000000000000 ) ;
#12884 = ORIENTED_EDGE ( 'NONE', *, *, #21494, .F. ) ;
#12885 = CARTESIAN_POINT ( 'NONE',  ( -2.672651547586948120E-15, -29.19062499938548427, 13.33755215474603162 ) ) ;
#12886 = DIRECTION ( 'NONE',  ( 0.000000000000000000, 0.000000000000000000, 1.000000000000000000 ) ) ;
#12887 = CARTESIAN_POINT ( 'NONE',  ( 3.959305671612554781E-15, 40.00000000000000000, 12.99999999999999289 ) ) ;
#12888 = CARTESIAN_POINT ( 'NONE',  ( -19.82388608118395013, 23.96296185032730364, -6.500000000000000000 ) ) ;
#12889 = CARTESIAN_POINT ( 'NONE',  ( 4.000000000000001776, 25.00000000000000000, 8.999999999999992895 ) ) ;
#12890 =( BOUNDED_CURVE ( )  B_SPLINE_CURVE ( 2, ( #16005, #21612, #23972, #6053, #23701, #25797, #15616, #11674, #19650 ),
 .UNSPECIFIED., .F., .F. ) 
 B_SPLINE_CURVE_WITH_KNOTS ( ( 3, 2, 2, 2, 3 ),
 ( 0.9250000000000000444, 0.9333333333333333481, 0.9499999999999999556, 0.9666666666666666741, 0.9749999999999999778 ),
 .UNSPECIFIED. ) 
 CURVE ( )  GEOMETRIC_REPRESENTATION_ITEM ( )  RATIONAL_B_SPLINE_CURVE ( ( 0.9330127018922194093, 0.9330127018922198534, 1.000000000000000000, 0.8660254037844387076, 1.000000000000000000, 0.8660254037844387076, 1.000000000000000000, 0.9330127018922194093, 0.9330127018922194093 ) ) 
 REPRESENTATION_ITEM ( '' )  );
#12891 = DIRECTION ( 'NONE',  ( 0.000000000000000000, 0.000000000000000000, 1.000000000000000000 ) ) ;
#12892 = VECTOR ( 'NONE', #18832, 1000.000000000000000 ) ;
#12893 = EDGE_CURVE ( 'NONE', #23600, #21660, #23365, .T. ) ;
#12894 = CARTESIAN_POINT ( 'NONE',  ( 1.071796769724495446, 25.54240381056767362, 4.999999999999992895 ) ) ;
#12895 = VECTOR ( 'NONE', #1816, 1000.000000000000000 ) ;
#12896 =( LENGTH_UNIT ( ) NAMED_UNIT ( * ) SI_UNIT ( .MILLI., .METRE. ) );
#12897 = CARTESIAN_POINT ( 'NONE',  ( 19.50730832598392084, 19.50730832598383913, 12.99999999999999289 ) ) ;
#12899 = ADVANCED_FACE ( 'NONE', ( #22053 ), #10156, .F. ) ;
#12898 = AXIS2_PLACEMENT_3D ( 'NONE', #10561, #22739, #18421 ) ;
#12900 = CARTESIAN_POINT ( 'NONE',  ( 19.82388608118411710, -23.96296185032715798, -6.500000000000000000 ) ) ;
#12901 = CARTESIAN_POINT ( 'NONE',  ( 18.56476993080373461, 20.08051945865570787, 4.999999999999992895 ) ) ;
#12902 = AXIS2_PLACEMENT_3D ( 'NONE', #24962, #3379, #25477 ) ;
#12903 = CARTESIAN_POINT ( 'NONE',  ( 1.071796769724494336, 25.35759618943234628, 12.99999999999999467 ) ) ;
#12904 = CARTESIAN_POINT ( 'NONE',  ( 22.97888821056449515, 17.66649345464567489, 8.999999999999992895 ) ) ;
#12905 = CARTESIAN_POINT ( 'NONE',  ( 20.40451381974352074, 17.74831644178408041, 12.25316411605952283 ) ) ;
#12906 = LINE ( 'NONE', #8716, #23483 ) ;
#12907 = DIRECTION ( 'NONE',  ( 1.000000000000000000, 0.000000000000000000, -0.000000000000000000 ) ) ;
#12908 = CARTESIAN_POINT ( 'NONE',  ( 1.878215178125004048, 28.36562499938548143, 5.746835883940462963 ) ) ;
#12909 = CARTESIAN_POINT ( 'NONE',  ( 3.834746474454188013E-15, 27.75624999877096855, 4.999999999999992006 ) ) ;
#12910 = CARTESIAN_POINT ( 'NONE',  ( 16.20808571844850121, 21.52048047436717937, 6.831223922626973533 ) ) ;
#12911 = DIRECTION ( 'NONE',  ( -0.5358267949789882190, 0.8443279255020205154, 0.000000000000000000 ) ) ;
#12912 = ORIENTED_EDGE ( 'NONE', *, *, #13425, .T. ) ;
#12913 = CYLINDRICAL_SURFACE ( 'NONE', #1327, 4.000000000000000000 ) ;
#12914 = CARTESIAN_POINT ( 'NONE',  ( 2.000000000000000888, 28.01874999877096784, 12.46410161513774817 ) ) ;
#12915 = CARTESIAN_POINT ( 'NONE',  ( 3.756430356249997882, -28.55312499938548498, 11.16877607737301226 ) ) ;
#12917 = VERTEX_POINT ( 'NONE', #18155 ) ;
#12916 = FACE_OUTER_BOUND ( 'NONE', #11534, .T. ) ;
#12918 = DIRECTION ( 'NONE',  ( 0.000000000000000000, 0.000000000000000000, -1.000000000000000000 ) ) ;
#12919 = EDGE_CURVE ( 'NONE', #4816, #24761, #14221, .T. ) ;
#12920 = AXIS2_PLACEMENT_3D ( 'NONE', #17093, #18663, #21024 ) ;
#12921 = VERTEX_POINT ( 'NONE', #12377 ) ;
#12922 = CARTESIAN_POINT ( 'NONE',  ( 3.756430356249997882, -27.20312499938548001, 11.16877607737301226 ) ) ;
#12923 = ORIENTED_EDGE ( 'NONE', *, *, #2367, .F. ) ;
#12924 = VERTEX_POINT ( 'NONE', #2823 ) ;
#12925 = FACE_OUTER_BOUND ( 'NONE', #17560, .T. ) ;
#12926 = CARTESIAN_POINT ( 'NONE',  ( -3.756430356249997882, 27.72812499938548569, 8.999999999999992895 ) ) ;
#12927 = AXIS2_PLACEMENT_3D ( 'NONE', #6165, #2126, #9837 ) ;
#12928 = AXIS2_PLACEMENT_3D ( 'NONE', #9142, #25104, #7193 ) ;
#12929 = CARTESIAN_POINT ( 'NONE',  ( -1.878215178124998497, -12.25316411605951927, 1.003124999385485161 ) ) ;
#12930 = SURFACE_STYLE_USAGE ( .BOTH. , #3121 ) ;
#12931 = CARTESIAN_POINT ( 'NONE',  ( -30.10000000000000142, 3.686186865433532535E-15, -6.500000000000000000 ) ) ;
#12932 = AXIS2_PLACEMENT_3D ( 'NONE', #25196, #3338, #3596 ) ;
#12933 = CARTESIAN_POINT ( 'NONE',  ( 2.672651547586948120E-15, 28.17812499938548143, 13.33755215474602984 ) ) ;
#12934 = CARTESIAN_POINT ( 'NONE',  ( -27.92360179968386547, -13.69242354489123770, -2.750000000000000000 ) ) ;
#12935 = CIRCLE ( 'NONE', #821, 31.10000000000000142 ) ;
#12936 = CARTESIAN_POINT ( 'NONE',  ( -5.532151103383211144, 34.50000000000000000, 11.32277940608570255 ) ) ;
#12937 = CARTESIAN_POINT ( 'NONE',  ( 3.735045420075836212E-15, 29.30312499938548498, 4.662447845253954171 ) ) ;
#12938 = DIRECTION ( 'NONE',  ( -1.000000000000000000, 0.000000000000000000, 0.000000000000000000 ) ) ;
#12939 = DIRECTION ( 'NONE',  ( 0.000000000000000000, 0.000000000000000000, -1.000000000000000000 ) ) ;
#12940 = DIRECTION ( 'NONE',  ( 0.000000000000000000, 0.000000000000000000, 1.000000000000000000 ) ) ;
#12941 = CYLINDRICAL_SURFACE ( 'NONE', #16374, 0.5000000000000004441 ) ;
#12942 = CARTESIAN_POINT ( 'NONE',  ( -1.878215178125000939, -26.97812499938548569, 12.25316411605952283 ) ) ;
#12943 = CARTESIAN_POINT ( 'NONE',  ( 1.878215178125004048, 26.22812499938548569, 5.746835883940462963 ) ) ;
#12944 = AXIS2_PLACEMENT_3D ( 'NONE', #18267, #22319, #12375 ) ;
#12945 = ADVANCED_FACE ( 'NONE', ( #16696 ), #20874, .F. ) ;
#12946 = CARTESIAN_POINT ( 'NONE',  ( -1.057460391440397258E-14, 29.55624999877096926, 4.999999999999992006 ) ) ;
#12948 = CARTESIAN_POINT ( 'NONE',  ( 0.000000000000000000, 0.000000000000000000, -6.500000000000000000 ) ) ;
#12947 = AXIS2_PLACEMENT_3D ( 'NONE', #16291, #1375, #15237 ) ;
#12949 = CARTESIAN_POINT ( 'NONE',  ( -1.859271017917182139E-15, -28.48749999999999716, 12.99999999999999289 ) ) ;
#12950 = ORIENTED_EDGE ( 'NONE', *, *, #8103, .F. ) ;
#12951 = CARTESIAN_POINT ( 'NONE',  ( 30.78811501957141772, -4.393401135981229721, -6.500000000000000000 ) ) ;
#12953 = VERTEX_POINT ( 'NONE', #18396 ) ;
#12952 = DIRECTION ( 'NONE',  ( 0.000000000000000000, 0.000000000000000000, 1.000000000000000000 ) ) ;
#12954 = EDGE_LOOP ( 'NONE', ( #22366, #18978 ) ) ;
#12955 = VECTOR ( 'NONE', #17774, 1000.000000000000000 ) ;
#12956 = ORIENTED_EDGE ( 'NONE', *, *, #3225, .F. ) ;
#12957 = ORIENTED_EDGE ( 'NONE', *, *, #3693, .T. ) ;
#12958 = ORIENTED_EDGE ( 'NONE', *, *, #24655, .T. ) ;
#12959 = DIRECTION ( 'NONE',  ( -0.000000000000000000, 0.000000000000000000, -1.000000000000000000 ) ) ;
#12960 = AXIS2_PLACEMENT_3D ( 'NONE', #9432, #17413, #19485 ) ;
#12961 = EDGE_LOOP ( 'NONE', ( #3289, #5028, #24584 ) ) ;
#12962 = FACE_OUTER_BOUND ( 'NONE', #11401, .T. ) ;
#12963 = CARTESIAN_POINT ( 'NONE',  ( 0.000000000000000000, 0.000000000000000000, -6.500000000000000000 ) ) ;
#12964 = AXIS2_PLACEMENT_3D ( 'NONE', #13357, #23670, #15706 ) ;
#12965 = CARTESIAN_POINT ( 'NONE',  ( 3.756430356250003655, -8.999999999999992895, 0.1406249993854830072 ) ) ;
#12966 = CARTESIAN_POINT ( 'NONE',  ( 2.000000000000003997, -5.535898384862238508, 0.4687499987709661808 ) ) ;
#12967 = CARTESIAN_POINT ( 'NONE',  ( 17.82559248041273037, 23.13798723633140142, 8.999999999999992895 ) ) ;
#12968 = CARTESIAN_POINT ( 'NONE',  ( -3.756430356249996994, 26.82812499938548711, 8.999999999999992895 ) ) ;
#12969 = CARTESIAN_POINT ( 'NONE',  ( 8.377607117416804527, -24.67207871933483787, 20.00001200000000168 ) ) ;
#12970 = CARTESIAN_POINT ( 'NONE',  ( -1.878215178124998497, -12.25316411605951927, 4.490624999385482319 ) ) ;
#12971 = DIRECTION ( 'NONE',  ( 0.1253332335643120576, 0.9921147013144768767, 0.000000000000000000 ) ) ;
#12972 = CARTESIAN_POINT ( 'NONE',  ( 21.21320343559646915, 21.21320343559638744, 8.999999999999992895 ) ) ;
#12973 = CARTESIAN_POINT ( 'NONE',  ( -4.648177544792955347E-16, 27.08124999877097139, 12.99999999999999289 ) ) ;
#12974 = CARTESIAN_POINT ( 'NONE',  ( -1.057460391440397258E-14, 29.16249999999999787, 4.999999999999992006 ) ) ;
#12975 =( BOUNDED_CURVE ( )  B_SPLINE_CURVE ( 2, ( #18072, #4186, #16366, #14651, #24332, #12163, #2484, #14400, #20384 ),
 .UNSPECIFIED., .F., .F. ) 
 B_SPLINE_CURVE_WITH_KNOTS ( ( 3, 2, 2, 2, 3 ),
 ( 0.6250000000000000000, 0.6333333333333333037, 0.6500000000000000222, 0.6666666666666666297, 0.6750000000000000444 ),
 .UNSPECIFIED. ) 
 CURVE ( )  GEOMETRIC_REPRESENTATION_ITEM ( )  RATIONAL_B_SPLINE_CURVE ( ( 0.9330127018922194093, 0.9330127018922194093, 1.000000000000000000, 0.8660254037844387076, 1.000000000000000000, 0.8660254037844387076, 1.000000000000000000, 0.9330127018922189652, 0.9330127018922194093 ) ) 
 REPRESENTATION_ITEM ( '' )  );
#12976 = CIRCLE ( 'NONE', #8380, 0.5000000000000004441 ) ;
#12977 = CARTESIAN_POINT ( 'NONE',  ( 1.878215178125004048, -5.746835883940462963, 4.378124999385484273 ) ) ;
#12978 = AXIS2_PLACEMENT_3D ( 'NONE', #13176, #21145, #3217 ) ;
#12979 = CARTESIAN_POINT ( 'NONE',  ( -20.20656826142300133, -23.64116323484216053, -6.500000000000000000 ) ) ;
#12980 = EDGE_CURVE ( 'NONE', #11742, #19703, #5260, .T. ) ;
#12981 = DIRECTION ( 'NONE',  ( 1.000000000000000000, 0.000000000000000000, 0.000000000000000000 ) ) ;
#12982 = ORIENTED_EDGE ( 'NONE', *, *, #14439, .T. ) ;
#12983 = CLOSED_SHELL ( 'NONE', ( #20116, #8531, #6455, #6974, #10177, #10948, #17461, #24835, #11843 ) ) ;
#12984 = ORIENTED_EDGE ( 'NONE', *, *, #23445, .T. ) ;
#12985 = CIRCLE ( 'NONE', #16326, 0.5000000000000000000 ) ;
#12986 = ADVANCED_FACE ( 'NONE', ( #6883 ), #4799, .T. ) ;
#12987 = ORIENTED_EDGE ( 'NONE', *, *, #8977, .T. ) ;
#12988 = CARTESIAN_POINT ( 'NONE',  ( 0.5000000000000000000, 0.000000000000000000, 19.50000000000000000 ) ) ;
#12989 = ORIENTED_EDGE ( 'NONE', *, *, #4988, .F. ) ;
#12990 = CARTESIAN_POINT ( 'NONE',  ( 1.878215178124995832, -25.85312499938548569, 5.746835883940462963 ) ) ;
#12991 = EDGE_CURVE ( 'NONE', #22105, #20014, #748, .T. ) ;
#12992 = ORIENTED_EDGE ( 'NONE', *, *, #24826, .T. ) ;
#12993 = DIRECTION ( 'NONE',  ( 1.000000000000000000, 0.000000000000000000, 0.000000000000000000 ) ) ;
#12994 = ORIENTED_EDGE ( 'NONE', *, *, #22581, .T. ) ;
#12995 = ADVANCED_FACE ( 'NONE', ( #4666, #6755 ), #496, .F. ) ;
#12996 = DIRECTION ( 'NONE',  ( 0.000000000000000000, 0.000000000000000000, 1.000000000000000000 ) ) ;
#12997 = CARTESIAN_POINT ( 'NONE',  ( 4.000000000000001776, 25.41250000000000142, 11.30940107675849760 ) ) ;
#12998 = DIRECTION ( 'NONE',  ( 0.000000000000000000, 0.000000000000000000, 1.000000000000000000 ) ) ;
#12999 = AXIS2_PLACEMENT_3D ( 'NONE', #1822, #18278, #2326 ) ;
#13000 = CARTESIAN_POINT ( 'NONE',  ( 4.000000000000003553, 26.35000000000000142, 8.999999999999992895 ) ) ;
#13001 = CARTESIAN_POINT ( 'NONE',  ( 18.87091222291601866, 18.87091222291595827, 12.99999999999999289 ) ) ;
#13002 = CARTESIAN_POINT ( 'NONE',  ( 17.58921741601718125, 20.24541479397648303, 5.746835883940462963 ) ) ;
#13003 = AXIS2_PLACEMENT_3D ( 'NONE', #1007, #22444, #12378 ) ;
#13004 = CYLINDRICAL_SURFACE ( 'NONE', #22571, 0.5000000000000004441 ) ;
#13005 = CARTESIAN_POINT ( 'NONE',  ( 4.000000000000003553, 25.03749999999999787, 6.690598923241489970 ) ) ;
#13006 = CARTESIAN_POINT ( 'NONE',  ( 16.28763523133199342, 21.60002998725066803, 6.831223922626973533 ) ) ;
#13007 = CARTESIAN_POINT ( 'NONE',  ( 0.000000000000000000, 0.000000000000000000, -6.500000000000000000 ) ) ;
#13008 = EDGE_LOOP ( 'NONE', ( #8736, #5898, #21116, #481 ) ) ;
#13009 = CARTESIAN_POINT ( 'NONE',  ( 4.000000000000002665, 27.68124999877097281, 6.690598923241489970 ) ) ;
#13010 = CIRCLE ( 'NONE', #18445, 0.5000000000000005551 ) ;
#13011 = CARTESIAN_POINT ( 'NONE',  ( -2.672651547586948120E-15, -28.17812499938548143, 13.33755215474603162 ) ) ;
#13012 = AXIS2_PLACEMENT_3D ( 'NONE', #21050, #13462, #5338 ) ;
#13013 = EDGE_CURVE ( 'NONE', #19667, #5148, #22112, .T. ) ;
#13014 = CARTESIAN_POINT ( 'NONE',  ( -3.999999999999996447, 27.02500000000000213, 8.999999999999992895 ) ) ;
#13015 = PRODUCT_DEFINITION ( 'UNKNOWN', '', #198, #7309 ) ;
#13016 = CARTESIAN_POINT ( 'NONE',  ( 3.735045420075836212E-15, 25.81562499938548783, 4.662447845253954171 ) ) ;
#13017 = LINE ( 'NONE', #9080, #25493 ) ;
#13019 = ORIENTED_EDGE ( 'NONE', *, *, #21668, .T. ) ;
#13018 = DIRECTION ( 'NONE',  ( 0.000000000000000000, 0.000000000000000000, 1.000000000000000000 ) ) ;
#13020 = ORIENTED_EDGE ( 'NONE', *, *, #308, .F. ) ;
#13021 = DIRECTION ( 'NONE',  ( 0.000000000000000000, -0.000000000000000000, -1.000000000000000000 ) ) ;
#13022 = VECTOR ( 'NONE', #11606, 1000.000000000000000 ) ;
#13023 = DIRECTION ( 'NONE',  ( -0.000000000000000000, 0.000000000000000000, -1.000000000000000000 ) ) ;
#13024 = ORIENTED_EDGE ( 'NONE', *, *, #12141, .T. ) ;
#13025 = ADVANCED_FACE ( 'NONE', ( #2702 ), #18921, .F. ) ;
#13026 = CARTESIAN_POINT ( 'NONE',  ( 0.000000000000000000, 0.000000000000000000, 20.00000000000000000 ) ) ;
#13027 = CARTESIAN_POINT ( 'NONE',  ( -3.756430356249997882, 29.41562499938548569, 8.999999999999992895 ) ) ;
#13028 = CARTESIAN_POINT ( 'NONE',  ( 4.006172263299091013E-15, 25.47812499938548925, 13.33755215474603162 ) ) ;
#13029 = EDGE_CURVE ( 'NONE', #13257, #9189, #14188, .T. ) ;
#13030 = CIRCLE ( 'NONE', #13446, 0.4999999999999999445 ) ;
#13031 = CARTESIAN_POINT ( 'NONE',  ( 0.7500000000000001110, 9.184850993605150903E-17, 15.00000000000000178 ) ) ;
#13032 = CARTESIAN_POINT ( 'NONE',  ( -3.756430356249998326, 29.45312499938549422, 11.16877607737301226 ) ) ;
#13033 = VECTOR ( 'NONE', #21845, 999.9999999999998863 ) ;
#13034 = VECTOR ( 'NONE', #1208, 1000.000000000000000 ) ;
#13035 = CARTESIAN_POINT ( 'NONE',  ( 25.98730014090442353, 17.08421000182768523, -6.500000000000000000 ) ) ;
#13036 = CARTESIAN_POINT ( 'NONE',  ( -8.217531866531430751, -29.99470236596023653, -6.500000000000000000 ) ) ;
#13037 = CIRCLE ( 'NONE', #10519, 0.4999999999999997224 ) ;
#13038 = CYLINDRICAL_SURFACE ( 'NONE', #22616, 4.000000000000000000 ) ;
#13039 = CARTESIAN_POINT ( 'NONE',  ( 3.756430356250002323, 26.45312499938548356, 11.16877607737301403 ) ) ;
#13040 = CARTESIAN_POINT ( 'NONE',  ( 19.73390110347460435, 18.21815157562248544, 4.999999999999989342 ) ) ;
#13041 = CARTESIAN_POINT ( 'NONE',  ( 18.14379053194667790, 23.45618528786534895, 8.999999999999992895 ) ) ;
#13042 = CARTESIAN_POINT ( 'NONE',  ( 19.87418373385361292, 17.21798635589416548, 5.746835883940462963 ) ) ;
#13043 = CARTESIAN_POINT ( 'NONE',  ( 3.469446951953614189E-15, -8.999999999999992895, 8.000000000000000000 ) ) ;
#13044 = CARTESIAN_POINT ( 'NONE',  ( 3.756430356250003655, 28.74062499938548498, 8.999999999999992895 ) ) ;
#13045 = CARTESIAN_POINT ( 'NONE',  ( 4.648177544792955347E-16, 28.48750000000000071, 12.99999999999999289 ) ) ;
#13046 = AXIS2_PLACEMENT_3D ( 'NONE', #3261, #11239, #1316 ) ;
#13047 = CARTESIAN_POINT ( 'NONE',  ( 19.12944813935283150, 19.12944813935275690, 4.662447845253954171 ) ) ;
#13048 = CARTESIAN_POINT ( 'NONE',  ( 22.66719175354223736, 17.01033750404978662, 11.30940107675849760 ) ) ;
#13049 = VERTEX_POINT ( 'NONE', #7005 ) ;
#13050 = DIRECTION ( 'NONE',  ( 0.000000000000000000, 0.000000000000000000, 1.000000000000000000 ) ) ;
#13051 = CARTESIAN_POINT ( 'NONE',  ( -3.999999999999996447, 27.41874999877096641, 8.999999999999992895 ) ) ;
#13052 = CARTESIAN_POINT ( 'NONE',  ( 1.878215178124998497, -28.14062499938548356, 12.25316411605951927 ) ) ;
#13054 = ORIENTED_EDGE ( 'NONE', *, *, #18264, .T. ) ;
#13053 = CYLINDRICAL_SURFACE ( 'NONE', #20444, 0.5000000000000004441 ) ;
#13055 = CIRCLE ( 'NONE', #5003, 0.4999999999999998335 ) ;
#13056 = CARTESIAN_POINT ( 'NONE',  ( -3.756430356249996105, 27.24062499938548498, 6.831223922626973533 ) ) ;
#13057 = VECTOR ( 'NONE', #6801, 1000.000000000000000 ) ;
#13058 = ORIENTED_EDGE ( 'NONE', *, *, #23271, .T. ) ;
#13059 = EDGE_CURVE ( 'NONE', #25447, #15051, #24805, .T. ) ;
#13060 = CARTESIAN_POINT ( 'NONE',  ( -3.756430356250003655, -29.19062499938548072, 8.999999999999992895 ) ) ;
#13061 = VERTEX_POINT ( 'NONE', #10663 ) ;
#13062 = VERTEX_POINT ( 'NONE', #18653 ) ;
#13063 = CARTESIAN_POINT ( 'NONE',  ( 0.000000000000000000, 0.000000000000000000, -6.500000000000000000 ) ) ;
#13064 = CARTESIAN_POINT ( 'NONE',  ( 1.878215178125003382, 26.67812499938548854, 5.746835883940462963 ) ) ;
#13065 = EDGE_CURVE ( 'NONE', #14663, #5872, #4587, .T. ) ;
#13066 = CARTESIAN_POINT ( 'NONE',  ( 0.000000000000000000, 0.000000000000000000, 20.00000000000000000 ) ) ;
#13067 = AXIS2_PLACEMENT_3D ( 'NONE', #3919, #4039, #12003 ) ;
#13068 = CARTESIAN_POINT ( 'NONE',  ( 3.756430356250002323, -11.16877607737301226, 3.815624999385482052 ) ) ;
#13069 = DIRECTION ( 'NONE',  ( 0.000000000000000000, 0.000000000000000000, 1.000000000000000000 ) ) ;
#13070 = CARTESIAN_POINT ( 'NONE',  ( 1.878215178125000939, 27.31562499938548427, 12.25316411605952283 ) ) ;
#13071 = AXIS2_PLACEMENT_3D ( 'NONE', #7732, #9820, #7852 ) ;
#13072 = CARTESIAN_POINT ( 'NONE',  ( -7.901901826148023498E-15, 28.71250000000000568, 4.999999999999992006 ) ) ;
#13073 = CYLINDRICAL_SURFACE ( 'NONE', #6326, 0.5000000000000004441 ) ;
#13074 = UNCERTAINTY_MEASURE_WITH_UNIT (LENGTH_MEASURE( 1.000000000000000082E-05 ), #2224, 'distance_accuracy_value', 'NONE');
#13075 = CARTESIAN_POINT ( 'NONE',  ( -3.756430356249997438, 28.55312499938548498, 11.16877607737301048 ) ) ;
#13076 = DIRECTION ( 'NONE',  ( 0.2486898871648653975, 0.9685831611286285225, 0.000000000000000000 ) ) ;
#13077 = DIRECTION ( 'NONE',  ( -0.000000000000000000, -1.000000000000000000, -0.000000000000000000 ) ) ;
#13078 = LINE ( 'NONE', #22877, #3438 ) ;
#13079 = CARTESIAN_POINT ( 'NONE',  ( 0.000000000000000000, 0.000000000000000000, 1.000000000000000000 ) ) ;
#13080 = CARTESIAN_POINT ( 'NONE',  ( 3.756430356249996994, -27.27812499938548640, 8.999999999999992895 ) ) ;
#13081 = CARTESIAN_POINT ( 'NONE',  ( -3.756430356249995661, 25.89062499938548356, 6.831223922626973533 ) ) ;
#13082 = CARTESIAN_POINT ( 'NONE',  ( 1.071796769724494558, 27.73615380933863861, 4.999999999999992895 ) ) ;
#13083 = VECTOR ( 'NONE', #9334, 1000.000000000000000 ) ;
#13084 = DIRECTION ( 'NONE',  ( -0.000000000000000000, -0.000000000000000000, 1.000000000000000000 ) ) ;
#13085 = CARTESIAN_POINT ( 'NONE',  ( -3.526711513754876570, 29.50000000000000000, 4.145898033750337497 ) ) ;
#13086 = ORIENTED_EDGE ( 'NONE', *, *, #9041, .T. ) ;
#13087 = DIRECTION ( 'NONE',  ( 0.000000000000000000, 1.000000000000000000, 0.000000000000000000 ) ) ;
#13089 = ORIENTED_EDGE ( 'NONE', *, *, #7830, .F. ) ;
#13088 = DIRECTION ( 'NONE',  ( 0.000000000000000000, 0.000000000000000000, -1.000000000000000000 ) ) ;
#13090 = AXIS2_PLACEMENT_3D ( 'NONE', #22285, #20709, #24623 ) ;
#13091 = EDGE_LOOP ( 'NONE', ( #3021, #19791, #19901, #6484 ) ) ;
#13092 = ORIENTED_EDGE ( 'NONE', *, *, #4197, .T. ) ;
#13093 = VERTEX_POINT ( 'NONE', #4523 ) ;
#13094 = ORIENTED_EDGE ( 'NONE', *, *, #19921, .F. ) ;
#13095 = EDGE_CURVE ( 'NONE', #18169, #10049, #20443, .T. ) ;
#13096 = LINE ( 'NONE', #7205, #2611 ) ;
#13097 = DIRECTION ( 'NONE',  ( -0.000000000000000000, -0.000000000000000000, 1.000000000000000000 ) ) ;
#13098 = CARTESIAN_POINT ( 'NONE',  ( -3.756430356249996105, 27.69062499938548072, 6.831223922626973533 ) ) ;
#13099 = EDGE_CURVE ( 'NONE', #10033, #1701, #12082, .T. ) ;
#13100 = COLOUR_RGB ( '',0.8941176470588234615, 0.8941176470588234615, 0.8941176470588234615 ) ;
#13101 = CARTESIAN_POINT ( 'NONE',  ( -1.878215178124998497, -12.25316411605951927, 4.603124999385483918 ) ) ;
#13102 = CARTESIAN_POINT ( 'NONE',  ( 3.752267015613588906E-15, -4.381197846482986158, 2.756249998770968102 ) ) ;
#13103 = DIRECTION ( 'NONE',  ( -1.000000000000000000, 0.000000000000000000, 0.000000000000000000 ) ) ;
#13104 = CIRCLE ( 'NONE', #16450, 0.5000000000000001110 ) ;
#13105 = CARTESIAN_POINT ( 'NONE',  ( 1.878215178125000939, 26.97812499938548569, 12.25316411605952283 ) ) ;
#13106 = EDGE_CURVE ( 'NONE', #10774, #5737, #1659, .T. ) ;
#13107 = AXIS2_PLACEMENT_3D ( 'NONE', #13066, #7033, #7175 ) ;
#13108 = CARTESIAN_POINT ( 'NONE',  ( -8.377607117416792093, -24.67207871933483787, 20.00001200000000168 ) ) ;
#13109 = CARTESIAN_POINT ( 'NONE',  ( -3.756430356249995661, -6.831223922626973533, 3.028124999385485072 ) ) ;
#13110 = CARTESIAN_POINT ( 'NONE',  ( -23.64116323484210369, 20.20656826142307949, -2.750000000000000000 ) ) ;
#13111 = FACE_OUTER_BOUND ( 'NONE', #20114, .T. ) ;
#13112 = CARTESIAN_POINT ( 'NONE',  ( -5.752022074721577560, 38.59074972337092646, 7.645898033750358813 ) ) ;
#13113 = CARTESIAN_POINT ( 'NONE',  ( 3.756430356250003655, -8.999999999999992895, 0.1968749993854837510 ) ) ;
#13114 = CARTESIAN_POINT ( 'NONE',  ( -3.756430356249996994, -8.999999999999992895, 3.628124999385483829 ) ) ;
#13115 = LINE ( 'NONE', #25265, #17464 ) ;
#13116 = LINE ( 'NONE', #5515, #17246 ) ;
#13117 = VERTEX_POINT ( 'NONE', #21514 ) ;
#13118 = ORIENTED_EDGE ( 'NONE', *, *, #2634, .F. ) ;
#13119 = ORIENTED_EDGE ( 'NONE', *, *, #25823, .T. ) ;
#13120 = CYLINDRICAL_SURFACE ( 'NONE', #5843, 6.000000000000000888 ) ;
#13121 = PRESENTATION_LAYER_ASSIGNMENT (  '', '', ( #16898 ) ) ;
#13122 = ORIENTED_EDGE ( 'NONE', *, *, #25683, .F. ) ;
#13123 = CARTESIAN_POINT ( 'NONE',  ( -3.756430356250003655, -25.25312499938548427, 8.999999999999992895 ) ) ;
#13124 = VERTEX_POINT ( 'NONE', #11314 ) ;
#13125 = CARTESIAN_POINT ( 'NONE',  ( 0.000000000000000000, 0.000000000000000000, -6.500000000000000000 ) ) ;
#13126 = ORIENTED_EDGE ( 'NONE', *, *, #5533, .T. ) ;
#13127 = CARTESIAN_POINT ( 'NONE',  ( -0.5000000000000000000, 0.000000000000000000, 19.50000000000000000 ) ) ;
#13128 =( BOUNDED_CURVE ( )  B_SPLINE_CURVE ( 2, ( #503, #2970, #2445, #10406, #18405, #14611, #2583, #8473, #12511 ),
 .UNSPECIFIED., .F., .F. ) 
 B_SPLINE_CURVE_WITH_KNOTS ( ( 3, 2, 2, 2, 3 ),
 ( 0.7249999999999999778, 0.7333333333333332815, 0.7500000000000000000, 0.7666666666666667185, 0.7750000000000000222 ),
 .UNSPECIFIED. ) 
 CURVE ( )  GEOMETRIC_REPRESENTATION_ITEM ( )  RATIONAL_B_SPLINE_CURVE ( ( 0.9330127018922194093, 0.9330127018922194093, 1.000000000000000000, 0.8660254037844387076, 1.000000000000000000, 0.8660254037844387076, 1.000000000000000000, 0.9330127018922194093, 0.9330127018922194093 ) ) 
 REPRESENTATION_ITEM ( '' )  );
#13129 = CARTESIAN_POINT ( 'NONE',  ( 3.756430356250004099, 28.77812499938548285, 6.831223922626973533 ) ) ;
#13130 = CARTESIAN_POINT ( 'NONE',  ( 3.834746474454188013E-15, 28.20624999877096428, 4.999999999999992006 ) ) ;
#13131 = EDGE_CURVE ( 'NONE', #939, #21627, #19295, .T. ) ;
#13132 = LINE ( 'NONE', #21101, #1301 ) ;
#13133 = LINE ( 'NONE', #18507, #17111 ) ;
#13134 = CARTESIAN_POINT ( 'NONE',  ( 17.05888733012726632, 19.71508470808657520, 12.25316411605951927 ) ) ;
#13135 =( BOUNDED_CURVE ( )  B_SPLINE_CURVE ( 2, ( #2618, #2097, #10578, #2475, #6141, #2234, #2354, #14265, #20377, #22232, #8507, #10065, #14511, #18574, #24450, #16488, #4315, #397, #271, #22482, #15972, #6405, #12410, #10445, #23937, #22353, #4564, #8366, #12291, #18440, #6528, #148, #535, #14395, #10191, #4179, #18187, #6020, #8239, #12545, #22090, #20523, #20257, #19992, #12157, #20132, #7984, #16215, #14125, #4437, #8119, #24058, #14001, #21972, #12015, #24185, #4047, #6274, #16094, #16357, #10310, #18304, #24325, #5218, #16996, #23139, #12687, #22755, #24843, #14644, #20657, #6656, #20917, #13196, #16740, #10831, #14903, #15170, #11096, #20781, #11214, #21168, #16878, #3240, #2739, #657, #21051, #24708, #2862, #3001, #6919, #13075, #22874, #1154, #10701, #7182, #8626, #17124, #9132, #4956, #18955, #22626, #8896, #18687, #24961, #5096, #3128, #16604, #15031, #24567, #1042, #12937, #19073, #25096, #775, #4714, #7044, #18825, #4832, #914, #8750 ),
 .UNSPECIFIED., .F., .F. ) 
 B_SPLINE_CURVE_WITH_KNOTS ( ( 3, 2, 2, 2, 2, 2, 2, 2, 2, 2, 2, 2, 2, 2, 2, 2, 2, 2, 2, 2, 2, 2, 2, 2, 2, 2, 2, 2, 2, 2, 2, 2, 2, 2, 2, 2, 2, 2, 2, 2, 2, 2, 2, 2, 2, 2, 2, 2, 2, 2, 2, 2, 2, 2, 2, 2, 2, 2, 2, 2, 3 ),
 ( 0.000000000000000000, 0.01666666666666666644, 0.03333333333333333287, 0.05000000000000000278, 0.06666666666666666574, 0.08333333333333332871, 0.1000000000000000056, 0.1166666666666666685, 0.1333333333333333315, 0.1499999999999999944, 0.1666666666666666574, 0.1833333333333333204, 0.2000000000000000111, 0.2166666666666666741, 0.2333333333333333370, 0.2500000000000000000, 0.2666666666666666630, 0.2833333333333333259, 0.2999999999999999889, 0.3166666666666666519, 0.3333333333333333148, 0.3499999999999999778, 0.3666666666666666408, 0.3833333333333333592, 0.4000000000000000222, 0.4166666666666666852, 0.4333333333333333481, 0.4500000000000000111, 0.4666666666666666741, 0.4833333333333333370, 0.5000000000000000000, 0.5166666666666667185, 0.5333333333333333259, 0.5500000000000000444, 0.5666666666666666519, 0.5833333333333333703, 0.5999999999999999778, 0.6166666666666666963, 0.6333333333333333037, 0.6500000000000000222, 0.6666666666666666297, 0.6833333333333333481, 0.6999999999999999556, 0.7166666666666666741, 0.7333333333333332815, 0.7500000000000000000, 0.7666666666666667185, 0.7833333333333333259, 0.8000000000000000444, 0.8166666666666666519, 0.8333333333333333703, 0.8499999999999999778, 0.8666666666666666963, 0.8833333333333333037, 0.9000000000000000222, 0.9166666666666666297, 0.9333333333333333481, 0.9499999999999999556, 0.9666666666666666741, 0.9833333333333332815, 1.000000000000000000 ),
 .UNSPECIFIED. ) 
 CURVE ( )  GEOMETRIC_REPRESENTATION_ITEM ( )  RATIONAL_B_SPLINE_CURVE ( ( 1.000000000000000000, 0.8660254037844387076, 1.000000000000000000, 0.8660254037844387076, 1.000000000000000000, 0.8660254037844387076, 1.000000000000000000, 0.8660254037844387076, 1.000000000000000000, 0.8660254037844387076, 1.000000000000000000, 0.8660254037844387076, 1.000000000000000000, 0.8660254037844387076, 1.000000000000000000, 0.8660254037844387076, 1.000000000000000000, 0.8660254037844387076, 1.000000000000000000, 0.8660254037844387076, 1.000000000000000000, 0.8660254037844387076, 1.000000000000000000, 0.8660254037844387076, 1.000000000000000000, 0.8660254037844387076, 1.000000000000000000, 0.8660254037844387076, 1.000000000000000000, 0.8660254037844387076, 1.000000000000000000, 0.8660254037844387076, 1.000000000000000000, 0.8660254037844387076, 1.000000000000000000, 0.8660254037844387076, 1.000000000000000000, 0.8660254037844387076, 1.000000000000000000, 0.8660254037844387076, 1.000000000000000000, 0.8660254037844387076, 1.000000000000000000, 0.8660254037844387076, 1.000000000000000000, 0.8660254037844387076, 1.000000000000000000, 0.8660254037844387076, 1.000000000000000000, 0.8660254037844387076, 1.000000000000000000, 0.8660254037844387076, 1.000000000000000000, 0.8660254037844387076, 1.000000000000000000, 0.8660254037844387076, 1.000000000000000000, 0.8660254037844387076, 1.000000000000000000, 0.8660254037844387076, 1.000000000000000000, 0.8660254037844387076, 1.000000000000000000, 0.8660254037844387076, 1.000000000000000000, 0.8660254037844387076, 1.000000000000000000, 0.8660254037844387076, 1.000000000000000000, 0.8660254037844387076, 1.000000000000000000, 0.8660254037844387076, 1.000000000000000000, 0.8660254037844387076, 1.000000000000000000, 0.8660254037844387076, 1.000000000000000000, 0.8660254037844387076, 1.000000000000000000, 0.8660254037844387076, 1.000000000000000000, 0.8660254037844387076, 1.000000000000000000, 0.8660254037844387076, 1.000000000000000000, 0.8660254037844387076, 1.000000000000000000, 0.8660254037844387076, 1.000000000000000000, 0.8660254037844387076, 1.000000000000000000, 0.8660254037844387076, 1.000000000000000000, 0.8660254037844387076, 1.000000000000000000, 0.8660254037844387076, 1.000000000000000000, 0.8660254037844387076, 1.000000000000000000, 0.8660254037844387076, 1.000000000000000000, 0.8660254037844387076, 1.000000000000000000, 0.8660254037844387076, 1.000000000000000000, 0.8660254037844387076, 1.000000000000000000, 0.8660254037844387076, 1.000000000000000000, 0.8660254037844387076, 1.000000000000000000, 0.8660254037844387076, 1.000000000000000000, 0.8660254037844387076, 1.000000000000000000, 0.8660254037844387076, 1.000000000000000000, 0.8660254037844387076, 1.000000000000000000, 0.8660254037844387076, 1.000000000000000000 ) ) 
 REPRESENTATION_ITEM ( '' )  );
#13136 = DIRECTION ( 'NONE',  ( 1.000000000000000000, 0.000000000000000000, 0.000000000000000000 ) ) ;
#13137 = ADVANCED_FACE ( 'NONE', ( #13165 ), #15253, .T. ) ;
#13138 = PRODUCT_DEFINITION_FORMATION_WITH_SPECIFIED_SOURCE ( 'ANY', '', #4426, .NOT_KNOWN. ) ;
#13139 = EDGE_CURVE ( 'NONE', #3323, #3258, #11448, .T. ) ;
#13140 = CARTESIAN_POINT ( 'NONE',  ( 3.752267015613588906E-15, 26.01249999999999929, 4.381197846482986158 ) ) ;
#13141 = CARTESIAN_POINT ( 'NONE',  ( 21.14924941424430571, 15.83685465832548900, 8.999999999999992895 ) ) ;
#13142 = DIRECTION ( 'NONE',  ( 0.000000000000000000, 0.000000000000000000, 1.000000000000000000 ) ) ;
#13143 = VERTEX_POINT ( 'NONE', #9366 ) ;
#13144 = EDGE_CURVE ( 'NONE', #4479, #15851, #20864, .T. ) ;
#13145 = ORIENTED_EDGE ( 'NONE', *, *, #11420, .F. ) ;
#13146 = CARTESIAN_POINT ( 'NONE',  ( -3.999999999999998224, 28.76874999877097139, 8.999999999999992895 ) ) ;
#13147 = DIRECTION ( 'NONE',  ( -0.3681245526846659843, 0.9297764858882561212, 0.000000000000000000 ) ) ;
#13148 = CARTESIAN_POINT ( 'NONE',  ( -1.071796769724485454, 27.11740381056766580, 12.99999999999999467 ) ) ;
#13149 = CARTESIAN_POINT ( 'NONE',  ( 3.756430356250002323, 27.46562499938548640, 11.16877607737301226 ) ) ;
#13150 = CARTESIAN_POINT ( 'NONE',  ( -0.7500000000000001110, 1.299038105676658450, 18.19999999999999929 ) ) ;
#13151 = ORIENTED_EDGE ( 'NONE', *, *, #13347, .F. ) ;
#13152 = ORIENTED_EDGE ( 'NONE', *, *, #23271, .F. ) ;
#13153 = DIRECTION ( 'NONE',  ( 0.000000000000000000, 0.000000000000000000, 1.000000000000000000 ) ) ;
#13154 = DIRECTION ( 'NONE',  ( -0.000000000000000000, -0.000000000000000000, -1.000000000000000000 ) ) ;
#13155 = ORIENTED_EDGE ( 'NONE', *, *, #4335, .F. ) ;
#13156 = EDGE_CURVE ( 'NONE', #11375, #13603, #25049, .T. ) ;
#13157 = CARTESIAN_POINT ( 'NONE',  ( -3.999999999999997335, 25.71249999999999503, 11.30940107675849404 ) ) ;
#13158 = CARTESIAN_POINT ( 'NONE',  ( 1.878215178125001605, 25.96562499938548996, 12.25316411605952283 ) ) ;
#13159 = CARTESIAN_POINT ( 'NONE',  ( -1.071796769724492338, -26.20134618820330275, 12.99999999999999467 ) ) ;
#13160 = CARTESIAN_POINT ( 'NONE',  ( 2.000000000000005329, 25.52500000000000568, 5.535898384862238508 ) ) ;
#13161 = EDGE_CURVE ( 'NONE', #13717, #5974, #19419, .T. ) ;
#13162 = DIRECTION ( 'NONE',  ( 1.000000000000000000, 0.000000000000000000, 0.000000000000000000 ) ) ;
#13163 = PRODUCT_CONTEXT ( 'NONE', #21129, 'mechanical' ) ;
#13164 = EDGE_CURVE ( 'NONE', #20076, #22016, #18364, .T. ) ;
#13165 = FACE_OUTER_BOUND ( 'NONE', #1417, .T. ) ;
#13166 = CARTESIAN_POINT ( 'NONE',  ( 3.469446951953614189E-15, 39.50000000000000000, 8.999999999999992895 ) ) ;
#13167 = CARTESIAN_POINT ( 'NONE',  ( -3.756430356249996105, 27.57812499938548356, 6.831223922626973533 ) ) ;
#13168 = DIRECTION ( 'NONE',  ( 0.8660254037844395958, 0.4999999999999982792, 0.000000000000000000 ) ) ;
#13169 = CARTESIAN_POINT ( 'NONE',  ( 15.35305598651295256, 21.00991023600526830, 11.30940107675849404 ) ) ;
#13170 = CARTESIAN_POINT ( 'NONE',  ( 23.96650046397252609, 18.30964621448006824, 8.999999999999992895 ) ) ;
#13171 = EDGE_CURVE ( 'NONE', #1111, #17932, #1638, .T. ) ;
#13172 = DIRECTION ( 'NONE',  ( 0.000000000000000000, 1.000000000000000000, 0.000000000000000000 ) ) ;
#13173 = CARTESIAN_POINT ( 'NONE',  ( 3.756430356250004099, 26.97812499938548569, 6.831223922626973533 ) ) ;
#13174 = CARTESIAN_POINT ( 'NONE',  ( 4.000000000000003553, -8.999999999999992895, 1.350000000000000533 ) ) ;
#13175 = CARTESIAN_POINT ( 'NONE',  ( 21.36138144860026600, 16.04898669268145639, 11.16877607737301403 ) ) ;
#13176 = CARTESIAN_POINT ( 'NONE',  ( 0.000000000000000000, 0.000000000000000000, -6.500000000000000000 ) ) ;
#13177 = ORIENTED_EDGE ( 'NONE', *, *, #21385, .F. ) ;
#13178 = CARTESIAN_POINT ( 'NONE',  ( 3.752267015613588906E-15, 26.40624999877097068, 4.381197846482986158 ) ) ;
#13179 = CARTESIAN_POINT ( 'NONE',  ( 4.000000000000003553, 28.09374999877097068, 8.999999999999992895 ) ) ;
#13180 = CARTESIAN_POINT ( 'NONE',  ( -1.878215178125004048, -28.36562499938548143, 5.746835883940462963 ) ) ;
#13182 = ORIENTED_EDGE ( 'NONE', *, *, #14434, .F. ) ;
#13181 = DIRECTION ( 'NONE',  ( -0.06279051952930156388, 0.9980267284282724471, 0.000000000000000000 ) ) ;
#13183 = CARTESIAN_POINT ( 'NONE',  ( 1.878215178125004048, 26.22812499938548569, 5.746835883940462963 ) ) ;
#13184 = ORIENTED_EDGE ( 'NONE', *, *, #16159, .T. ) ;
#13185 = CARTESIAN_POINT ( 'NONE',  ( -1.878215178125004048, -27.01562499938548711, 5.746835883940462963 ) ) ;
#13186 = ORIENTED_EDGE ( 'NONE', *, *, #9319, .T. ) ;
#13187 = VERTEX_POINT ( 'NONE', #15135 ) ;
#13188 = DIRECTION ( 'NONE',  ( 1.000000000000000000, 0.000000000000000000, 0.000000000000000000 ) ) ;
#13189 = CARTESIAN_POINT ( 'NONE',  ( 0.000000000000000000, 27.84062499938548996, 13.33755215474602984 ) ) ;
#13190 = CARTESIAN_POINT ( 'NONE',  ( -3.756430356249996994, -8.999999999999992895, 1.715624999385483074 ) ) ;
#13191 = CARTESIAN_POINT ( 'NONE',  ( 4.000000000000003553, 28.99374999877096926, 8.999999999999992895 ) ) ;
#13192 = SURFACE_SIDE_STYLE ('',( #9648 ) ) ;
#13193 = DIRECTION ( 'NONE',  ( -0.000000000000000000, 1.000000000000000000, -0.000000000000000000 ) ) ;
#13194 = LINE ( 'NONE', #19454, #25502 ) ;
#13195 = CARTESIAN_POINT ( 'NONE',  ( 3.469446951953614189E-15, -8.999999999999992895, 0.000000000000000000 ) ) ;
#13196 = CARTESIAN_POINT ( 'NONE',  ( 3.756430356250003211, 27.87812499938548427, 6.831223922626973533 ) ) ;
#13197 = CARTESIAN_POINT ( 'NONE',  ( -1.999999999999995781, 26.89374999877097139, 5.535898384862237620 ) ) ;
#13198 = LINE ( 'NONE', #3242, #7035 ) ;
#13199 = FACE_OUTER_BOUND ( 'NONE', #11605, .T. ) ;
#13200 = EDGE_CURVE ( 'NONE', #17442, #8421, #16280, .T. ) ;
#13201 = DIRECTION ( 'NONE',  ( -0.000000000000000000, -1.000000000000000000, -0.000000000000000000 ) ) ;
#13202 = CARTESIAN_POINT ( 'NONE',  ( 3.756430356249997882, -28.21562499938548285, 11.16877607737301226 ) ) ;
#13203 = CARTESIAN_POINT ( 'NONE',  ( 0.5000000000000000000, 6.000000000000000000, 19.50000000000000000 ) ) ;
#13204 = ADVANCED_FACE ( 'NONE', ( #17595 ), #21015, .T. ) ;
#13205 = DIRECTION ( 'NONE',  ( 0.000000000000000000, 0.000000000000000000, -1.000000000000000000 ) ) ;
#13206 = CARTESIAN_POINT ( 'NONE',  ( 1.859271017917182139E-15, 26.18124999877096570, 12.99999999999999289 ) ) ;
#13207 = CARTESIAN_POINT ( 'NONE',  ( 21.04646806692120009, 19.53071853906906341, 4.999999999999997335 ) ) ;
#13208 = VERTEX_POINT ( 'NONE', #14990 ) ;
#13209 = DIRECTION ( 'NONE',  ( -0.000000000000000000, 1.000000000000000000, -0.000000000000000000 ) ) ;
#13211 = ORIENTED_EDGE ( 'NONE', *, *, #16872, .T. ) ;
#13210 = CARTESIAN_POINT ( 'NONE',  ( 0.000000000000000000, 0.000000000000000000, 1.000000000000000000 ) ) ;
#13212 = EDGE_CURVE ( 'NONE', #10117, #674, #2498, .T. ) ;
#13213 = ORIENTED_EDGE ( 'NONE', *, *, #2505, .F. ) ;
#13214 = EDGE_CURVE ( 'NONE', #13512, #421, #11060, .T. ) ;
#13215 = VERTEX_POINT ( 'NONE', #7393 ) ;
#13216 = VERTEX_POINT ( 'NONE', #13036 ) ;
#13217 = ORIENTED_EDGE ( 'NONE', *, *, #17469, .T. ) ;
#13218 = CARTESIAN_POINT ( 'NONE',  ( 17.87326343783925253, -25.45105997952931176, -6.500000000000000000 ) ) ;
#13219 = CARTESIAN_POINT ( 'NONE',  ( -1.999999999999998224, 29.29374999877096997, 12.46410161513774639 ) ) ;
#13220 = CARTESIAN_POINT ( 'NONE',  ( 23.59283907696195115, 18.53082671639309353, 10.80044967790456845 ) ) ;
#13221 = CARTESIAN_POINT ( 'NONE',  ( -1.878215178124995832, -5.746835883940462963, 4.003124999385484273 ) ) ;
#13222 = CARTESIAN_POINT ( 'NONE',  ( 2.000000000000003997, -5.535898384862238508, 0.9187499987709686344 ) ) ;
#13223 = DIRECTION ( 'NONE',  ( 1.000000000000000000, 0.000000000000000000, 0.000000000000000000 ) ) ;
#13224 = DIRECTION ( 'NONE',  ( 0.000000000000000000, 1.000000000000000000, 0.000000000000000000 ) ) ;
#13225 = CARTESIAN_POINT ( 'NONE',  ( -1.071796769724491227, -26.83615380933863293, 4.999999999999989342 ) ) ;
#13226 = CARTESIAN_POINT ( 'NONE',  ( 21.21320343559646915, 21.21320343559638744, 8.999999999999992895 ) ) ;
#13227 = CARTESIAN_POINT ( 'NONE',  ( -3.999999999999997335, -11.30940107675849404, 0.2624999999999988454 ) ) ;
#13228 = DIRECTION ( 'NONE',  ( 0.000000000000000000, 0.000000000000000000, 1.000000000000000000 ) ) ;
#13229 = CARTESIAN_POINT ( 'NONE',  ( 0.000000000000000000, 0.000000000000000000, -6.500000000000000000 ) ) ;
#13230 = FACE_OUTER_BOUND ( 'NONE', #2121, .T. ) ;
#13231 = CARTESIAN_POINT ( 'NONE',  ( -4.000000000000001776, -26.70624999877097139, 11.30940107675849760 ) ) ;
#13232 = FACE_OUTER_BOUND ( 'NONE', #14247, .T. ) ;
#13233 = EDGE_CURVE ( 'NONE', #4650, #22072, #21293, .T. ) ;
#13234 = CARTESIAN_POINT ( 'NONE',  ( -28.14012133169306296, 13.24173596767408867, -6.500000000000000000 ) ) ;
#13235 = MANIFOLD_SOLID_BREP ( 'Extrude-Thin1', #17985 ) ;
#13236 = CARTESIAN_POINT ( 'NONE',  ( -3.999999999999996447, -8.999999999999992895, 4.218749998770966236 ) ) ;
#13237 = ORIENTED_EDGE ( 'NONE', *, *, #25353, .F. ) ;
#13238 = CARTESIAN_POINT ( 'NONE',  ( 0.000000000000000000, 31.10000000000000142, -6.500000000000000000 ) ) ;
#13239 = EDGE_LOOP ( 'NONE', ( #25491, #18672, #15434, #1378 ) ) ;
#13240 = VERTEX_POINT ( 'NONE', #2024 ) ;
#13241 = PLANE ( 'NONE',  #17906 ) ;
#13242 = ORIENTED_EDGE ( 'NONE', *, *, #11382, .T. ) ;
#13243 = DIRECTION ( 'NONE',  ( -0.000000000000000000, 0.000000000000000000, 1.000000000000000000 ) ) ;
#13244 = ORIENTED_EDGE ( 'NONE', *, *, #17901, .F. ) ;
#13245 = CARTESIAN_POINT ( 'NONE',  ( -24.86329371854755266, 18.68225429291749151, 1.000000000000000000 ) ) ;
#13246 = EDGE_CURVE ( 'NONE', #9331, #9030, #16639, .T. ) ;
#13247 = ORIENTED_EDGE ( 'NONE', *, *, #7122, .T. ) ;
#13248 = CARTESIAN_POINT ( 'NONE',  ( -1.999999999999998224, 27.55000000000000071, 12.46410161513774639 ) ) ;
#13249 = CARTESIAN_POINT ( 'NONE',  ( 7.248980000274197977, 30.24338421796781518, 1.000000000000000000 ) ) ;
#13250 = FACE_OUTER_BOUND ( 'NONE', #6990, .T. ) ;
#13251 = CARTESIAN_POINT ( 'NONE',  ( 5.112995299272250684E-15, 25.56250000000000711, 4.999999999999992006 ) ) ;
#13252 = CARTESIAN_POINT ( 'NONE',  ( 15.65123912826409480, 20.96363388418277296, 6.831223922626973533 ) ) ;
#13253 = CARTESIAN_POINT ( 'NONE',  ( 7.734255490826784651, -30.12293631110048153, -6.500000000000000000 ) ) ;
#13254 = CARTESIAN_POINT ( 'NONE',  ( 3.752267015613588906E-15, 25.11250000000000071, 4.381197846482986158 ) ) ;
#13255 = CARTESIAN_POINT ( 'NONE',  ( 17.90741546755112523, 20.56361284551042701, 5.746835883940462963 ) ) ;
#13256 = LINE ( 'NONE', #15347, #16667 ) ;
#13257 = VERTEX_POINT ( 'NONE', #3986 ) ;
#13258 = ORIENTED_EDGE ( 'NONE', *, *, #15387, .F. ) ;
#13259 = CARTESIAN_POINT ( 'NONE',  ( -1.999999999999996669, 27.94374999877097565, 12.46410161513774639 ) ) ;
#13260 = CARTESIAN_POINT ( 'NONE',  ( -3.469446951953614189E-15, -30.00000000000000355, 8.999999999999992895 ) ) ;
#13261 = EDGE_LOOP ( 'NONE', ( #8004, #4263, #3527, #964 ) ) ;
#13262 = LINE ( 'NONE', #3318, #3721 ) ;
#13263 = EDGE_CURVE ( 'NONE', #6150, #14821, #3308, .T. ) ;
#13264 = CARTESIAN_POINT ( 'NONE',  ( -3.756430356249995661, 28.14062499938548356, 6.831223922626973533 ) ) ;
#13265 = DIRECTION ( 'NONE',  ( 1.000000000000000000, 0.000000000000000000, -0.000000000000000000 ) ) ;
#13266 = ORIENTED_EDGE ( 'NONE', *, *, #22155, .F. ) ;
#13267 = ORIENTED_EDGE ( 'NONE', *, *, #13425, .F. ) ;
#13268 =( BOUNDED_CURVE ( )  B_SPLINE_CURVE ( 2, ( #13280, #8982, #11173, #24925, #25673, #22966, #21254, #1753, #9723 ),
 .UNSPECIFIED., .F., .F. ) 
 B_SPLINE_CURVE_WITH_KNOTS ( ( 3, 2, 2, 2, 3 ),
 ( 0.7750000000000000222, 0.7833333333333333259, 0.8000000000000000444, 0.8166666666666666519, 0.8250000000000000666 ),
 .UNSPECIFIED. ) 
 CURVE ( )  GEOMETRIC_REPRESENTATION_ITEM ( )  RATIONAL_B_SPLINE_CURVE ( ( 0.9330127018922194093, 0.9330127018922194093, 1.000000000000000000, 0.8660254037844387076, 1.000000000000000000, 0.8660254037844387076, 1.000000000000000000, 0.9330127018922189652, 0.9330127018922194093 ) ) 
 REPRESENTATION_ITEM ( '' )  );
#13269 = FACE_OUTER_BOUND ( 'NONE', #1980, .T. ) ;
#13270 = CIRCLE ( 'NONE', #14575, 31.10000000000000142 ) ;
#13271 = MANIFOLD_SOLID_BREP ( 'Boss-Extrude2', #12983 ) ;
#13272 = CARTESIAN_POINT ( 'NONE',  ( 27.49048467073848911, -14.54246377227368647, -2.750000000000000000 ) ) ;
#13273 = ORIENTED_EDGE ( 'NONE', *, *, #1206, .T. ) ;
#13274 = CARTESIAN_POINT ( 'NONE',  ( -3.735045420075836212E-15, -28.96562499938548640, 4.662447845253954171 ) ) ;
#13275 = CARTESIAN_POINT ( 'NONE',  ( -3.756430356249995661, 25.32812499938548356, 6.831223922626973533 ) ) ;
#13276 =( BOUNDED_CURVE ( )  B_SPLINE_CURVE ( 2, ( #21815, #12257, #5985, #10161, #236, #6108, #10402, #22198, #14092 ),
 .UNSPECIFIED., .F., .F. ) 
 B_SPLINE_CURVE_WITH_KNOTS ( ( 3, 2, 2, 2, 3 ),
 ( 0.2250000000000000056, 0.2333333333333333370, 0.2500000000000000000, 0.2666666666666666630, 0.2750000000000000222 ),
 .UNSPECIFIED. ) 
 CURVE ( )  GEOMETRIC_REPRESENTATION_ITEM ( )  RATIONAL_B_SPLINE_CURVE ( ( 0.9330127018922194093, 0.9330127018922194093, 1.000000000000000000, 0.8660254037844387076, 1.000000000000000000, 0.8660254037844387076, 1.000000000000000000, 0.9330127018922191873, 0.9330127018922194093 ) ) 
 REPRESENTATION_ITEM ( '' )  );
#13277 = CARTESIAN_POINT ( 'NONE',  ( -3.756430356249997882, 26.26562499938548711, 8.999999999999992895 ) ) ;
#13278 = CARTESIAN_POINT ( 'NONE',  ( -1.859271017917182139E-15, -26.18124999877096570, 12.99999999999999289 ) ) ;
#13279 = CARTESIAN_POINT ( 'NONE',  ( 1.878215178125005158, 28.81562499938548783, 5.746835883940462963 ) ) ;
#13280 = CARTESIAN_POINT ( 'NONE',  ( 1.394453263437886604E-15, 28.88124999877097210, 12.99999999999999289 ) ) ;
#13281 = PRODUCT_CONTEXT ( 'NONE', #15297, 'mechanical' ) ;
#13282 = CARTESIAN_POINT ( 'NONE',  ( 3.469446951953614189E-15, -8.999999999999992895, 18.00000000000000000 ) ) ;
#13283 = DIRECTION ( 'NONE',  ( -0.000000000000000000, -1.000000000000000000, -0.000000000000000000 ) ) ;
#13284 = AXIS2_PLACEMENT_3D ( 'NONE', #442, #18609, #16132 ) ;
#13285 = CARTESIAN_POINT ( 'NONE',  ( 2.672651547586948120E-15, 27.27812499938548640, 13.33755215474603162 ) ) ;
#13286 = CARTESIAN_POINT ( 'NONE',  ( -1.294650675951837693, -29.97301818707614984, 5.206367449752296039 ) ) ;
#13287 = CARTESIAN_POINT ( 'NONE',  ( 23.27056975780394765, 17.95817500188513094, 11.16877607737301226 ) ) ;
#13288 = CARTESIAN_POINT ( 'NONE',  ( 20.32269083260512588, 20.32269083260505838, 13.33755215474602984 ) ) ;
#13289 = CARTESIAN_POINT ( 'NONE',  ( 24.27856662945507438, 19.43607991388980238, -2.750000000000000000 ) ) ;
#13290 = CARTESIAN_POINT ( 'NONE',  ( 3.756430356250002323, 27.35312499938547859, 11.16877607737301226 ) ) ;
#13291 = DIRECTION ( 'NONE',  ( 0.000000000000000000, 0.000000000000000000, 1.000000000000000000 ) ) ;
#13292 = ADVANCED_FACE ( 'NONE', ( #15760 ), #21637, .F. ) ;
#13293 = CARTESIAN_POINT ( 'NONE',  ( 18.78246010926947918, 21.43865748722877740, 5.746835883940462963 ) ) ;
#13294 = CARTESIAN_POINT ( 'NONE',  ( 21.33252770405263732, 18.50410057930636754, 5.535898384862238508 ) ) ;
#13295 = AXIS2_PLACEMENT_3D ( 'NONE', #537, #18689, #16490 ) ;
#13296 = ORIENTED_EDGE ( 'NONE', *, *, #19247, .F. ) ;
#13297 = CARTESIAN_POINT ( 'NONE',  ( 4.000000000000003553, 25.43124999877096926, 6.690598923241489970 ) ) ;
#13298 = CARTESIAN_POINT ( 'NONE',  ( -3.999999999999997335, 29.25624999877096499, 11.30940107675849404 ) ) ;
#13299 = CARTESIAN_POINT ( 'NONE',  ( -3.756430356250003655, -29.64062499938548356, 8.999999999999992895 ) ) ;
#13301 = VERTEX_POINT ( 'NONE', #23725 ) ;
#13300 = CARTESIAN_POINT ( 'NONE',  ( 1.859271017917182139E-15, 25.78750000000000142, 12.99999999999999289 ) ) ;
#13302 = CARTESIAN_POINT ( 'NONE',  ( 3.756430356250002323, 26.11562499938548498, 11.16877607737301403 ) ) ;
#13303 = EDGE_CURVE ( 'NONE', #10526, #13848, #16520, .T. ) ;
#13304 = CARTESIAN_POINT ( 'NONE',  ( -22.56362157461194329, 13.02991752792602931, 20.00001200000000168 ) ) ;
#13305 = CARTESIAN_POINT ( 'NONE',  ( 3.756430356249996994, -28.06562499938548427, 8.999999999999992895 ) ) ;
#13306 = VERTEX_POINT ( 'NONE', #4599 ) ;
#13307 = ORIENTED_EDGE ( 'NONE', *, *, #14470, .T. ) ;
#13308 = EDGE_CURVE ( 'NONE', #15503, #3397, #20885, .T. ) ;
#13309 = SURFACE_SIDE_STYLE ('',( #23244 ) ) ;
#13310 = CARTESIAN_POINT ( 'NONE',  ( 3.756430356250004543, 26.64062499938549067, 6.831223922626973533 ) ) ;
#13311 = CIRCLE ( 'NONE', #16653, 0.4999999999999998335 ) ;
#13312 = CIRCLE ( 'NONE', #2027, 0.5000000000000013323 ) ;
#13313 = CARTESIAN_POINT ( 'NONE',  ( 3.756430356250003655, -8.999999999999992895, 0.1406249993854830072 ) ) ;
#13314 = EDGE_CURVE ( 'NONE', #13377, #18495, #7656, .T. ) ;
#13315 = AXIS2_PLACEMENT_3D ( 'NONE', #4357, #10111, #16530 ) ;
#13316 = VECTOR ( 'NONE', #23561, 1000.000000000000000 ) ;
#13317 = CARTESIAN_POINT ( 'NONE',  ( -30.24338421796790044, -7.248980000273874680, -2.750000000000000000 ) ) ;
#13318 = DIRECTION ( 'NONE',  ( 0.000000000000000000, 0.000000000000000000, 1.000000000000000000 ) ) ;
#13319 = LINE ( 'NONE', #20220, #10891 ) ;
#13320 = FACE_OUTER_BOUND ( 'NONE', #4818, .T. ) ;
#13321 = CARTESIAN_POINT ( 'NONE',  ( 29.99470236596029693, -8.217531866531192719, 1.000000000000000000 ) ) ;
#13322 = CARTESIAN_POINT ( 'NONE',  ( 4.000000000000003553, 25.88124999877096855, 6.690598923241489970 ) ) ;
#13323 = CARTESIAN_POINT ( 'NONE',  ( -7.234255490827218082, -30.12293631110037140, -6.500000000000000000 ) ) ;
#13324 = CYLINDRICAL_SURFACE ( 'NONE', #25150, 31.10000000000000142 ) ;
#13325 = CARTESIAN_POINT ( 'NONE',  ( -1.071796769724481901, 27.56740381056766864, 12.99999999999999645 ) ) ;
#13326 = CARTESIAN_POINT ( 'NONE',  ( -3.756430356250003655, -28.85312499938548569, 8.999999999999992895 ) ) ;
#13327 = CARTESIAN_POINT ( 'NONE',  ( 3.756430356250003655, 25.25312499938548427, 8.999999999999992895 ) ) ;
#13328 = CYLINDRICAL_SURFACE ( 'NONE', #1617, 4.000000000000000000 ) ;
#13329 = VECTOR ( 'NONE', #22494, 1000.000000000000000 ) ;
#13330 = CARTESIAN_POINT ( 'NONE',  ( 18.71181319714904490, 18.71181319714897739, 4.999999999999991118 ) ) ;
#13331 = CARTESIAN_POINT ( 'NONE',  ( 20.30280345481879323, 20.30280345481869730, 4.999999999999992006 ) ) ;
#13333 = ORIENTED_EDGE ( 'NONE', *, *, #5886, .F. ) ;
#13332 = CIRCLE ( 'NONE', #23293, 0.4999999999999997224 ) ;
#13334 = LINE ( 'NONE', #21310, #18858 ) ;
#13335 = CARTESIAN_POINT ( 'NONE',  ( -14.54246377227378062, -27.49048467073843227, -2.750000000000000000 ) ) ;
#13337 = EDGE_LOOP ( 'NONE', ( #15043, #12068, #22427, #7441 ) ) ;
#13336 = CARTESIAN_POINT ( 'NONE',  ( -27.25313774936430633, -14.98253926456308172, 1.000000000000000000 ) ) ;
#13338 = AXIS2_PLACEMENT_3D ( 'NONE', #16590, #14626, #2721 ) ;
#13339 = VERTEX_POINT ( 'NONE', #8654 ) ;
#13341 = ORIENTED_EDGE ( 'NONE', *, *, #13161, .F. ) ;
#13340 = AXIS2_PLACEMENT_3D ( 'NONE', #19845, #1690, #1945 ) ;
#13342 = ORIENTED_EDGE ( 'NONE', *, *, #308, .T. ) ;
#13343 = PRODUCT_RELATED_PRODUCT_CATEGORY ( 'part', '', ( #24254 ) ) ;
#13344 = ORIENTED_EDGE ( 'NONE', *, *, #12078, .F. ) ;
#13345 = CYLINDRICAL_SURFACE ( 'NONE', #25568, 31.10000000000000142 ) ;
#13346 = CARTESIAN_POINT ( 'NONE',  ( 1.500000000000001776, -10.49999999999999289, 30.00000000000000355 ) ) ;
#13347 = EDGE_CURVE ( 'NONE', #23094, #3781, #2090, .T. ) ;
#13348 = CARTESIAN_POINT ( 'NONE',  ( -1.999999999999998224, 28.00000000000000711, 12.46410161513774639 ) ) ;
#13349 = AXIS2_PLACEMENT_3D ( 'NONE', #14359, #10023, #18023 ) ;
#13350 = ADVANCED_FACE ( 'NONE', ( #9045 ), #7217, .F. ) ;
#13351 = CARTESIAN_POINT ( 'NONE',  ( 1.878215178125000939, -12.25316411605952283, 0.9656249993854824076 ) ) ;
#13352 = CARTESIAN_POINT ( 'NONE',  ( -1.999999999999995781, -5.535898384862237620, 1.893749998770968723 ) ) ;
#13353 = CARTESIAN_POINT ( 'NONE',  ( 0.000000000000000000, 0.000000000000000000, 0.000000000000000000 ) ) ;
#13354 =( BOUNDED_CURVE ( )  B_SPLINE_CURVE ( 2, ( #3403, #11629, #5361, #9681, #1571, #25252, #13348, #11766, #25501 ),
 .UNSPECIFIED., .F., .F. ) 
 B_SPLINE_CURVE_WITH_KNOTS ( ( 3, 2, 2, 2, 3 ),
 ( 0.6250000000000000000, 0.6333333333333333037, 0.6500000000000000222, 0.6666666666666666297, 0.6750000000000000444 ),
 .UNSPECIFIED. ) 
 CURVE ( )  GEOMETRIC_REPRESENTATION_ITEM ( )  RATIONAL_B_SPLINE_CURVE ( ( 0.9330127018922194093, 0.9330127018922194093, 1.000000000000000000, 0.8660254037844387076, 1.000000000000000000, 0.8660254037844387076, 1.000000000000000000, 0.9330127018922189652, 0.9330127018922194093 ) ) 
 REPRESENTATION_ITEM ( '' )  );
#13355 = CARTESIAN_POINT ( 'NONE',  ( -3.756430356249995661, 25.44062499938548427, 6.831223922626973533 ) ) ;
#13356 = CIRCLE ( 'NONE', #1230, 31.10000000000000142 ) ;
#13357 = CARTESIAN_POINT ( 'NONE',  ( -31.03863125411927371, -1.952785157361310198, 1.000000000000000000 ) ) ;
#13358 = CARTESIAN_POINT ( 'NONE',  ( 25.99307600111999150, -0.5999999999999996447, 19.00000000000000000 ) ) ;
#13359 = CIRCLE ( 'NONE', #20871, 31.10000000000000142 ) ;
#13360 = CARTESIAN_POINT ( 'NONE',  ( -1.999999999999998224, -12.46410161513774639, 1.649999999999998579 ) ) ;
#13361 = CARTESIAN_POINT ( 'NONE',  ( 3.469446951953614189E-15, 40.00000000000000000, 8.999999999999992895 ) ) ;
#13362 = CYLINDRICAL_SURFACE ( 'NONE', #15792, 0.5000000000000004441 ) ;
#13363 = CARTESIAN_POINT ( 'NONE',  ( -3.999999999999996447, -8.999999999999992895, 0.000000000000000000 ) ) ;
#13364 = CARTESIAN_POINT ( 'NONE',  ( -2.000000000000000888, -28.01874999877096784, 12.46410161513774817 ) ) ;
#13365 = CARTESIAN_POINT ( 'NONE',  ( -1.878215178124998497, -12.25316411605951927, 3.253124999385483829 ) ) ;
#13366 = CARTESIAN_POINT ( 'NONE',  ( 3.834746474454188013E-15, 27.75624999877096855, 4.999999999999992006 ) ) ;
#13367 = DIRECTION ( 'NONE',  ( 0.000000000000000000, 0.000000000000000000, -1.000000000000000000 ) ) ;
#13368 = CARTESIAN_POINT ( 'NONE',  ( 15.41874213889403578, 27.00874656207305691, 1.000000000000000000 ) ) ;
#13369 = EDGE_LOOP ( 'NONE', ( #20328, #7958, #454, #6812 ) ) ;
#13370 = LINE ( 'NONE', #13507, #21288 ) ;
#13371 = EDGE_LOOP ( 'NONE', ( #14366, #19662, #861, #16893 ) ) ;
#13372 = AXIS2_PLACEMENT_3D ( 'NONE', #12581, #20561, #2650 ) ;
#13373 = ORIENTED_EDGE ( 'NONE', *, *, #19950, .T. ) ;
#13374 = FACE_OUTER_BOUND ( 'NONE', #6449, .T. ) ;
#13375 = ORIENTED_EDGE ( 'NONE', *, *, #5804, .F. ) ;
#13376 = CARTESIAN_POINT ( 'NONE',  ( -3.756430356250003655, -27.05312499938548498, 8.999999999999992895 ) ) ;
#13377 = VERTEX_POINT ( 'NONE', #24745 ) ;
#13378 = CARTESIAN_POINT ( 'NONE',  ( 2.000000000000000888, 26.72500000000000142, 12.46410161513774817 ) ) ;
#13379 = AXIS2_PLACEMENT_3D ( 'NONE', #10155, #16175, #24140 ) ;
#13380 = ADVANCED_FACE ( 'NONE', ( #24994 ), #18864, .T. ) ;
#13381 = ORIENTED_EDGE ( 'NONE', *, *, #17409, .F. ) ;
#13382 = CARTESIAN_POINT ( 'NONE',  ( 3.752267015613588906E-15, 27.81250000000000000, 4.381197846482986158 ) ) ;
#13383 = LINE ( 'NONE', #25668, #16838 ) ;
#13384 = EDGE_CURVE ( 'NONE', #5285, #2848, #14812, .T. ) ;
#13385 = CARTESIAN_POINT ( 'NONE',  ( -19.32388608118446527, -23.96296185032687376, 1.000000000000000000 ) ) ;
#13386 = CARTESIAN_POINT ( 'NONE',  ( -1.999999999999993117, 25.60000000000000497, 5.535898384862237620 ) ) ;
#13387 = CARTESIAN_POINT ( 'NONE',  ( 23.66831732222138740, 18.35592256630256003, 11.16877607737301226 ) ) ;
#13388 = AXIS2_PLACEMENT_3D ( 'NONE', #16997, #7045, #12688 ) ;
#13389 = VECTOR ( 'NONE', #24818, 1000.000000000000000 ) ;
#13390 = CARTESIAN_POINT ( 'NONE',  ( 4.000000000000003553, 26.35000000000000142, 8.999999999999992895 ) ) ;
#13391 = CLOSED_SHELL ( 'NONE', ( #23377, #5051, #24362, #21588, #23018, #3144, #24892, #1238, #5798, #18036, #23325, #24282, #20502, #18328 ) ) ;
#13392 = VECTOR ( 'NONE', #21196, 1000.000000000000000 ) ;
#13393 = EDGE_CURVE ( 'NONE', #4850, #3500, #18718, .T. ) ;
#13394 = CARTESIAN_POINT ( 'NONE',  ( 18.33167953626305646, 20.98787691422236179, 12.25316411605951927 ) ) ;
#13395 = DIRECTION ( 'NONE',  ( 1.000000000000000000, 0.000000000000000000, 0.000000000000000000 ) ) ;
#13396 = VERTEX_POINT ( 'NONE', #18986 ) ;
#13397 = ORIENTED_EDGE ( 'NONE', *, *, #12571, .T. ) ;
#13398 = CARTESIAN_POINT ( 'NONE',  ( -3.999999999999996447, 27.38124999877097210, 6.690598923241487306 ) ) ;
#13399 = CARTESIAN_POINT ( 'NONE',  ( -3.756430356250003211, -29.22812499938548569, 6.831223922626973533 ) ) ;
#13400 = VERTEX_POINT ( 'NONE', #7080 ) ;
#13401 = DIRECTION ( 'NONE',  ( 0.000000000000000000, 0.000000000000000000, 1.000000000000000000 ) ) ;
#13402 = CARTESIAN_POINT ( 'NONE',  ( -3.756430356249995661, 28.59062499938548640, 6.831223922626973533 ) ) ;
#13403 = DIRECTION ( 'NONE',  ( 1.000000000000000000, 0.000000000000000000, -0.000000000000000000 ) ) ;
#13404 = ORIENTED_EDGE ( 'NONE', *, *, #12222, .T. ) ;
#13405 = ORIENTED_EDGE ( 'NONE', *, *, #1321, .T. ) ;
#13406 = CARTESIAN_POINT ( 'NONE',  ( -27.25313774936397948, 14.98253926456367502, -6.500000000000000000 ) ) ;
#13407 = CIRCLE ( 'NONE', #6304, 0.5000000000000003331 ) ;
#13408 = VECTOR ( 'NONE', #432, 1000.000000000000000 ) ;
#13409 = CARTESIAN_POINT ( 'NONE',  ( 23.68807716974937705, 18.03122292025692275, 8.999999999999992895 ) ) ;
#13410 = ORIENTED_EDGE ( 'NONE', *, *, #4828, .F. ) ;
#13411 = AXIS2_PLACEMENT_3D ( 'NONE', #24011, #20463, #484 ) ;
#13412 = CARTESIAN_POINT ( 'NONE',  ( -2.672651547586948120E-15, -28.29062499938548925, 13.33755215474603162 ) ) ;
#13413 = EDGE_CURVE ( 'NONE', #16293, #11588, #952, .T. ) ;
#13414 = FACE_OUTER_BOUND ( 'NONE', #11288, .T. ) ;
#13415 = CARTESIAN_POINT ( 'NONE',  ( 3.756430356250002323, 27.35312499938548569, 11.16877607737301403 ) ) ;
#13416 = AXIS2_PLACEMENT_3D ( 'NONE', #20095, #13834, #18025 ) ;
#13417 = B_SPLINE_CURVE_WITH_KNOTS ( 'NONE', 3,
 ( #6730, #24123, #22560, #2552, #605, #2683, #18374, #2805, #475, #4257, #4644, #8444, #16674, #16160, #849, #4502 ),
 .UNSPECIFIED., .F., .F.,
 ( 4, 2, 2, 2, 2, 2, 2, 4 ),
 ( 2.789812634830972505E-07, 0.0002322844908106880453, 0.0004642900003578929839, 0.0006962955099050979497, 0.0009283010194523028070, 0.001160306528999507664, 0.001392312038546712847, 0.001856323057641127115 ),
 .UNSPECIFIED. ) ;
#13418 = DIRECTION ( 'NONE',  ( 0.000000000000000000, 1.000000000000000000, 0.000000000000000000 ) ) ;
#13419 = CARTESIAN_POINT ( 'NONE',  ( -3.999999999999996447, 27.06250000000000711, 11.30940107675849404 ) ) ;
#13420 = B_SPLINE_CURVE_WITH_KNOTS ( 'NONE', 3,
 ( #9785, #23909, #6377, #19962, #17765, #25734, #10034, #2066, #7817, #15798, #18032, #118, #13841, #1941, #4674, #2831 ),
 .UNSPECIFIED., .F., .F.,
 ( 4, 2, 2, 2, 2, 2, 2, 4 ),
 ( 2.789812634831446314E-07, 0.0002322844908106895361, 0.0004642900003578959655, 0.0006962955099051023949, 0.0009283010194523087701, 0.001160306528999515037, 0.001392312038546721521, 0.001856323057641130585 ),
 .UNSPECIFIED. ) ;
#13421 = EDGE_CURVE ( 'NONE', #20933, #25179, #7111, .T. ) ;
#13422 = CARTESIAN_POINT ( 'NONE',  ( -1.071796769724490117, 26.93259618943234202, 4.999999999999992895 ) ) ;
#13423 = AXIS2_PLACEMENT_3D ( 'NONE', #17995, #84, #8056 ) ;
#13424 = AXIS2_PLACEMENT_3D ( 'NONE', #14479, #24417, #22722 ) ;
#13425 = EDGE_CURVE ( 'NONE', #12921, #20210, #16706, .T. ) ;
#13426 = FACE_OUTER_BOUND ( 'NONE', #8276, .T. ) ;
#13427 = CARTESIAN_POINT ( 'NONE',  ( 3.756430356250003655, 26.49062499938548498, 8.999999999999992895 ) ) ;
#13428 = LINE ( 'NONE', #7522, #5370 ) ;
#13429 = CARTESIAN_POINT ( 'NONE',  ( 22.23415261606371374, 19.57795523810426630, 12.25316411605952283 ) ) ;
#13430 = CARTESIAN_POINT ( 'NONE',  ( 23.40315227927642283, 18.09075752335759901, 6.831223922626973533 ) ) ;
#13431 = DIRECTION ( 'NONE',  ( 0.000000000000000000, 0.000000000000000000, 1.000000000000000000 ) ) ;
#13432 =( BOUNDED_CURVE ( )  B_SPLINE_CURVE ( 2, ( #150, #8121, #16096, #11640, #24060, #18189, #4049, #17920, #6143 ),
 .UNSPECIFIED., .F., .F. ) 
 B_SPLINE_CURVE_WITH_KNOTS ( ( 3, 2, 2, 2, 3 ),
 ( 0.02500000000000000139, 0.03333333333333333287, 0.05000000000000000278, 0.06666666666666666574, 0.07500000000000001110 ),
 .UNSPECIFIED. ) 
 CURVE ( )  GEOMETRIC_REPRESENTATION_ITEM ( )  RATIONAL_B_SPLINE_CURVE ( ( 0.9330127018922194093, 0.9330127018922194093, 1.000000000000000000, 0.8660254037844387076, 1.000000000000000000, 0.8660254037844387076, 1.000000000000000000, 0.9330127018922191873, 0.9330127018922192983 ) ) 
 REPRESENTATION_ITEM ( '' )  );
#13433 = PLANE ( 'NONE',  #23993 ) ;
#13434 = AXIS2_PLACEMENT_3D ( 'NONE', #22586, #16842, #10399 ) ;
#13435 = CARTESIAN_POINT ( 'NONE',  ( 1.859271017917182139E-15, 26.68750000000000000, 12.99999999999999289 ) ) ;
#13436 = CARTESIAN_POINT ( 'NONE',  ( 21.67957950013421353, 16.36718474421539682, 11.16877607737301403 ) ) ;
#13437 = CARTESIAN_POINT ( 'NONE',  ( 4.000000000000002665, 25.80624999877096926, 11.30940107675849760 ) ) ;
#13438 = ORIENTED_EDGE ( 'NONE', *, *, #16426, .T. ) ;
#13439 = DIRECTION ( 'NONE',  ( 0.000000000000000000, -0.000000000000000000, 1.000000000000000000 ) ) ;
#13440 = CARTESIAN_POINT ( 'NONE',  ( 3.756430356250003655, 26.15312499938548640, 8.999999999999992895 ) ) ;
#13441 = CARTESIAN_POINT ( 'NONE',  ( -4.000000000000003553, -25.90000000000000213, 8.999999999999992895 ) ) ;
#13443 = ORIENTED_EDGE ( 'NONE', *, *, #14964, .F. ) ;
#13442 = CARTESIAN_POINT ( 'NONE',  ( 3.756430356250002323, 25.66562499938548925, 11.16877607737301403 ) ) ;
#13444 = CARTESIAN_POINT ( 'NONE',  ( 3.756430356250002323, 27.01562499938548356, 11.16877607737301403 ) ) ;
#13445 =( BOUNDED_CURVE ( )  B_SPLINE_CURVE ( 2, ( #14900, #22481, #12544, #24960, #20375, #4562, #22352 ),
 .UNSPECIFIED., .F., .F. ) 
 B_SPLINE_CURVE_WITH_KNOTS ( ( 3, 2, 2, 3 ),
 ( 0.7999999999999999334, 0.8166666666666665408, 0.8333333333333332593, 0.8499999999999998668 ),
 .UNSPECIFIED. ) 
 CURVE ( )  GEOMETRIC_REPRESENTATION_ITEM ( )  RATIONAL_B_SPLINE_CURVE ( ( 1.000000000000000888, 0.8660254037844378194, 1.000000000000000000, 0.8660254037844387076, 1.000000000000000000, 0.8660254037844395958, 0.9999999999999991118 ) ) 
 REPRESENTATION_ITEM ( '' )  );
#13446 = AXIS2_PLACEMENT_3D ( 'NONE', #17615, #25593, #5970 ) ;
#13447 = ORIENTED_EDGE ( 'NONE', *, *, #4563, .T. ) ;
#13448 = CARTESIAN_POINT ( 'NONE',  ( -3.735045420075836212E-15, -28.85312499938548569, 4.662447845253954171 ) ) ;
#13449 = ORIENTED_EDGE ( 'NONE', *, *, #5684, .F. ) ;
#13450 = VERTEX_POINT ( 'NONE', #23045 ) ;
#13451 = CARTESIAN_POINT ( 'NONE',  ( 18.97562471959685126, 23.23703773337175349, 6.356496494711869616 ) ) ;
#13452 = VECTOR ( 'NONE', #2031, 1000.000000000000000 ) ;
#13453 = CARTESIAN_POINT ( 'NONE',  ( 4.006172263299091013E-15, 25.25312499938549138, 4.662447845253954171 ) ) ;
#13454 = CIRCLE ( 'NONE', #15110, 0.4999999999999998335 ) ;
#13455 = CARTESIAN_POINT ( 'NONE',  ( 1.878215178125004048, -5.746835883940462963, 1.565624999385482274 ) ) ;
#13456 = ADVANCED_FACE ( 'NONE', ( #21081 ), #3157, .F. ) ;
#13457 = CARTESIAN_POINT ( 'NONE',  ( -1.878215178124998497, -12.25316411605951927, 4.153124999385485516 ) ) ;
#13458 = CARTESIAN_POINT ( 'NONE',  ( -2.000000000000000888, -27.17500000000000071, 12.46410161513774817 ) ) ;
#13459 = EDGE_CURVE ( 'NONE', #4812, #14631, #1262, .T. ) ;
#13460 = CARTESIAN_POINT ( 'NONE',  ( 28.72825533807129261, -11.91206721063050189, 1.000000000000000000 ) ) ;
#13461 = AXIS2_PLACEMENT_3D ( 'NONE', #1568, #5492, #25115 ) ;
#13462 = DIRECTION ( 'NONE',  ( 0.000000000000000000, 0.000000000000000000, 1.000000000000000000 ) ) ;
#13463 = CARTESIAN_POINT ( 'NONE',  ( 1.859271017917182139E-15, 28.48749999999999716, 12.99999999999999289 ) ) ;
#13464 = CYLINDRICAL_SURFACE ( 'NONE', #9221, 4.000000000000000000 ) ;
#13465 = CARTESIAN_POINT ( 'NONE',  ( -3.137519842735244810E-15, 27.30624999877096926, 4.999999999999991118 ) ) ;
#13466 = CARTESIAN_POINT ( 'NONE',  ( 21.39439954740644723, 15.73754529791400181, 11.30940107675849760 ) ) ;
#13467 = VERTEX_POINT ( 'NONE', #6830 ) ;
#13468 = DIRECTION ( 'NONE',  ( 0.000000000000000000, 0.000000000000000000, -1.000000000000000000 ) ) ;
#13469 = CARTESIAN_POINT ( 'NONE',  ( 3.756430356249996994, -28.17812499938548498, 8.999999999999992895 ) ) ;
#13470 = VECTOR ( 'NONE', #1966, 1000.000000000000000 ) ;
#13471 = CARTESIAN_POINT ( 'NONE',  ( -1.878215178124995832, 28.55312499938548498, 5.746835883940462963 ) ) ;
#13472 = CIRCLE ( 'NONE', #2189, 6.000000000000000000 ) ;
#13473 = DIRECTION ( 'NONE',  ( 0.000000000000000000, 0.000000000000000000, -1.000000000000000000 ) ) ;
#13474 = CARTESIAN_POINT ( 'NONE',  ( 2.000000000000000888, 27.17500000000000071, 12.46410161513774817 ) ) ;
#13475 = CARTESIAN_POINT ( 'NONE',  ( 30.78811501957144969, 4.393401135981008565, -2.750000000000000000 ) ) ;
#13476 = ORIENTED_EDGE ( 'NONE', *, *, #16826, .F. ) ;
#13477 = CARTESIAN_POINT ( 'NONE',  ( 1.878215178125003382, 29.37812499938548783, 5.746835883940462963 ) ) ;
#13478 = EDGE_CURVE ( 'NONE', #24860, #22793, #20033, .T. ) ;
#13479 = CARTESIAN_POINT ( 'NONE',  ( 7.248980000274102942, -30.24338421796783649, 1.000000000000000000 ) ) ;
#13481 = VERTEX_POINT ( 'NONE', #16910 ) ;
#13480 = CARTESIAN_POINT ( 'NONE',  ( 0.000000000000000000, 0.000000000000000000, -6.500000000000000000 ) ) ;
#13482 = ORIENTED_EDGE ( 'NONE', *, *, #17345, .F. ) ;
#13483 = VERTEX_POINT ( 'NONE', #24876 ) ;
#13484 = ORIENTED_EDGE ( 'NONE', *, *, #6435, .F. ) ;
#13485 = ORIENTED_EDGE ( 'NONE', *, *, #24866, .T. ) ;
#13486 = DIRECTION ( 'NONE',  ( 0.000000000000000000, 0.000000000000000000, 1.000000000000000000 ) ) ;
#13487 = CARTESIAN_POINT ( 'NONE',  ( -3.079592406726821441, 38.55544002051693298, 14.08467396235847069 ) ) ;
#13488 = CIRCLE ( 'NONE', #2198, 31.10000000000000142 ) ;
#13489 = ADVANCED_FACE ( 'NONE', ( #22907 ), #4993, .F. ) ;
#13490 = DIRECTION ( 'NONE',  ( 0.000000000000000000, 0.000000000000000000, 1.000000000000000000 ) ) ;
#13491 = CARTESIAN_POINT ( 'NONE',  ( 3.756430356250003655, -8.999999999999992895, 2.840624999385484184 ) ) ;
#13492 = CARTESIAN_POINT ( 'NONE',  ( 4.000000000000003553, -8.999999999999992895, 1.743749998770967924 ) ) ;
#13493 = CARTESIAN_POINT ( 'NONE',  ( 3.756430356250003655, 27.50312499938548427, 8.999999999999992895 ) ) ;
#13494 = CARTESIAN_POINT ( 'NONE',  ( 3.137519842735244810E-15, -26.85624999877096641, 4.999999999999991118 ) ) ;
#13495 = ADVANCED_BREP_SHAPE_REPRESENTATION ( '', ( #14010, #21036 ), #2676 ) ;
#13496 = CARTESIAN_POINT ( 'NONE',  ( 2.620986760973688460E-15, -13.61880215351699874, 0.7875000000000005329 ) ) ;
#13497 = CARTESIAN_POINT ( 'NONE',  ( 30.63887302793247969, 5.335677986744675749, -2.750000000000000000 ) ) ;
#13498 = DIRECTION ( 'NONE',  ( 0.000000000000000000, 0.000000000000000000, 1.000000000000000000 ) ) ;
#13499 = EDGE_CURVE ( 'NONE', #7472, #24402, #438, .T. ) ;
#13500 = CARTESIAN_POINT ( 'NONE',  ( -2.620986760973688460E-15, -27.08124999877096784, 13.61880215351699874 ) ) ;
#13501 = CARTESIAN_POINT ( 'NONE',  ( -3.756430356249996105, -6.831223922626973533, 4.490624999385483207 ) ) ;
#13502 = CARTESIAN_POINT ( 'NONE',  ( -29.57785765677936851, -9.610428525060582317, 1.000000000000000000 ) ) ;
#13503 = FACE_OUTER_BOUND ( 'NONE', #11501, .T. ) ;
#13504 = CARTESIAN_POINT ( 'NONE',  ( -3.999999999999995559, 25.63749999999999929, 6.690598923241487306 ) ) ;
#13505 = ORIENTED_EDGE ( 'NONE', *, *, #23557, .T. ) ;
#13506 = EDGE_CURVE ( 'NONE', #11885, #12101, #25066, .T. ) ;
#13507 = CARTESIAN_POINT ( 'NONE',  ( 27.00874656207294322, -15.41874213889423828, -2.750000000000000000 ) ) ;
#13508 = ORIENTED_EDGE ( 'NONE', *, *, #6598, .F. ) ;
#13509 = ADVANCED_FACE ( 'NONE', ( #690 ), #16635, .F. ) ;
#13510 = ORIENTED_EDGE ( 'NONE', *, *, #14907, .F. ) ;
#13511 = CYLINDRICAL_SURFACE ( 'NONE', #17069, 4.000000000000000000 ) ;
#13512 = VERTEX_POINT ( 'NONE', #25644 ) ;
#13513 = CARTESIAN_POINT ( 'NONE',  ( 3.756430356249997882, -28.21562499938548285, 11.16877607737301226 ) ) ;
#13514 = EDGE_LOOP ( 'NONE', ( #8002, #4874, #15692, #25219 ) ) ;
#13515 = DIRECTION ( 'NONE',  ( -0.000000000000000000, 0.000000000000000000, 1.000000000000000000 ) ) ;
#13516 = ORIENTED_EDGE ( 'NONE', *, *, #14403, .F. ) ;
#13518 = CARTESIAN_POINT ( 'NONE',  ( 4.000000000000001776, 26.76249999999999929, 11.30940107675849760 ) ) ;
#13517 = SHAPE_REPRESENTATION ( 'spindle', ( #21036 ), #7676 ) ;
#13519 = CARTESIAN_POINT ( 'NONE',  ( 3.063240906311874401, 29.84319947910909931, 11.57226653943513028 ) ) ;
#13520 = DIRECTION ( 'NONE',  ( 0.000000000000000000, 0.000000000000000000, 1.000000000000000000 ) ) ;
#13521 = CARTESIAN_POINT ( 'NONE',  ( 3.959305671612554781E-15, 30.00000000000000355, 12.99999999999999289 ) ) ;
#13522 = CARTESIAN_POINT ( 'NONE',  ( 17.26874589022832751, 22.58114064614699856, 8.999999999999992895 ) ) ;
#13523 = B_SPLINE_CURVE_WITH_KNOTS ( 'NONE', 3,
 ( #4446, #24458, #20387, #12418, #544, #4575, #6537, #12817, #4722, #12553, #280, #16224, #2243, #10198, #20533, #8248, #10587, #18581, #665, #6664, #12695, #1164, #25354, #16888, #3139, #18966, #10983, #19206, #5481, #2870, #9286, #9410, #21177, #9143 ),
 .UNSPECIFIED., .F., .F.,
 ( 4, 2, 2, 2, 2, 2, 2, 2, 2, 2, 2, 2, 2, 2, 2, 2, 4 ),
 ( 0.000000000000000000, 0.0007824850735655043557, 0.001564970147131008711, 0.002347455220696513176, 0.003129940294262017423, 0.003912425367827521670, 0.004694910441393026351, 0.005477395514958530165, 0.006259880588524034846, 0.007042365662089539527, 0.007824850735655043341, 0.008607335809220547154, 0.009389820882786052703, 0.01017230595635155652, 0.01095479102991706033, 0.01173727610348256588, 0.01251976117704806969 ),
 .UNSPECIFIED. ) ;
#13524 = CYLINDRICAL_SURFACE ( 'NONE', #1285, 4.000000000000000000 ) ;
#13525 = CARTESIAN_POINT ( 'NONE',  ( 3.752267015613588906E-15, 25.56250000000000000, 4.381197846482986158 ) ) ;
#13526 = CARTESIAN_POINT ( 'NONE',  ( 23.03192121915348878, 17.71952646323466496, 11.16877607737301403 ) ) ;
#13527 = CARTESIAN_POINT ( 'NONE',  ( 4.000000000000005329, 28.18750000000000000, 6.690598923241489970 ) ) ;
#13528 = ORIENTED_EDGE ( 'NONE', *, *, #24765, .T. ) ;
#13529 = EDGE_CURVE ( 'NONE', #19798, #13339, #8774, .T. ) ;
#13530 = ORIENTED_EDGE ( 'NONE', *, *, #11449, .T. ) ;
#13531 = CARTESIAN_POINT ( 'NONE',  ( 2.000000000000005329, 26.81874999877097210, 5.535898384862238508 ) ) ;
#13532 = ADVANCED_FACE ( 'NONE', ( #7725 ), #5750, .F. ) ;
#13533 = VECTOR ( 'NONE', #18650, 1000.000000000000000 ) ;
#13534 = VERTEX_POINT ( 'NONE', #15451 ) ;
#13535 = CARTESIAN_POINT ( 'NONE',  ( -7.734255490826573265, 30.12293631110053838, 1.000000000000000000 ) ) ;
#13536 = CARTESIAN_POINT ( 'NONE',  ( -1.878215178124995832, 29.00312499938548427, 5.746835883940462963 ) ) ;
#13537 = CARTESIAN_POINT ( 'NONE',  ( -3.999999999999995559, 27.38124999877096855, 6.690598923241487306 ) ) ;
#13538 = ORIENTED_EDGE ( 'NONE', *, *, #25028, .T. ) ;
#13539 = ORIENTED_EDGE ( 'NONE', *, *, #11589, .T. ) ;
#13540 = EDGE_CURVE ( 'NONE', #130, #20899, #22829, .T. ) ;
#13541 = CARTESIAN_POINT ( 'NONE',  ( -22.67092431280563503, 21.28941499438250062, -6.500000000000000000 ) ) ;
#13542 = EDGE_LOOP ( 'NONE', ( #4021, #18849, #5204, #5179 ) ) ;
#13543 = CARTESIAN_POINT ( 'NONE',  ( 3.162936011776061651, 38.99381541083456426, 4.492646367981153688 ) ) ;
#13544 = LINE ( 'NONE', #23336, #2192 ) ;
#13545 = CARTESIAN_POINT ( 'NONE',  ( -3.756430356249996549, 28.47812499938548569, 6.831223922626973533 ) ) ;
#13546 =( BOUNDED_CURVE ( )  B_SPLINE_CURVE ( 2, ( #7651, #15638, #24110, #9744, #10125, #13796, #71, #19674, #23862 ),
 .UNSPECIFIED., .F., .F. ) 
 B_SPLINE_CURVE_WITH_KNOTS ( ( 3, 2, 2, 2, 3 ),
 ( 0.3750000000000000000, 0.3833333333333333592, 0.4000000000000000222, 0.4166666666666666852, 0.4250000000000000444 ),
 .UNSPECIFIED. ) 
 CURVE ( )  GEOMETRIC_REPRESENTATION_ITEM ( )  RATIONAL_B_SPLINE_CURVE ( ( 0.9330127018922194093, 0.9330127018922194093, 1.000000000000000000, 0.8660254037844387076, 1.000000000000000000, 0.8660254037844387076, 1.000000000000000000, 0.9330127018922191873, 0.9330127018922194093 ) ) 
 REPRESENTATION_ITEM ( '' )  );
#13547 = CARTESIAN_POINT ( 'NONE',  ( 21.21320343559646915, 21.21320343559638744, 4.999999999999992006 ) ) ;
#13548 = CARTESIAN_POINT ( 'NONE',  ( 0.000000000000000000, 27.13750000000000639, 13.61880215351699874 ) ) ;
#13549 = CARTESIAN_POINT ( 'NONE',  ( -3.756430356249995661, 27.57812499938548356, 6.831223922626973533 ) ) ;
#13550 = DIRECTION ( 'NONE',  ( 0.000000000000000000, -1.000000000000000000, 0.000000000000000000 ) ) ;
#13551 = CYLINDRICAL_SURFACE ( 'NONE', #8408, 0.5000000000000004441 ) ;
#13552 = CARTESIAN_POINT ( 'NONE',  ( 3.756430356250003655, 27.84062499938548640, 8.999999999999992895 ) ) ;
#13553 = CARTESIAN_POINT ( 'NONE',  ( 19.18911027444996975, 19.18911027444990225, 13.61880215351699874 ) ) ;
#13554 = CARTESIAN_POINT ( 'NONE',  ( 16.60583328286593741, 21.91822803878461201, 6.831223922626973533 ) ) ;
#13555 = EDGE_CURVE ( 'NONE', #20939, #1141, #4604, .T. ) ;
#13556 = CARTESIAN_POINT ( 'NONE',  ( 18.70297436238422506, 21.53140148713034208, 12.46410161513774639 ) ) ;
#13557 = CARTESIAN_POINT ( 'NONE',  ( -3.137519842735244810E-15, 26.85624999877096641, 4.999999999999991118 ) ) ;
#13559 = ADVANCED_FACE ( 'NONE', ( #1718 ), #5371, .T. ) ;
#13558 = PLANE ( 'NONE',  #7052 ) ;
#13560 = DIRECTION ( 'NONE',  ( 0.000000000000000000, -1.000000000000000000, -0.000000000000000000 ) ) ;
#13561 = DIRECTION ( 'NONE',  ( 0.000000000000000000, 0.000000000000000000, -1.000000000000000000 ) ) ;
#13562 = ORIENTED_EDGE ( 'NONE', *, *, #20462, .T. ) ;
#13563 = CARTESIAN_POINT ( 'NONE',  ( 21.43417430471724927, 15.77732005522480563, 11.30940107675849760 ) ) ;
#13564 = CARTESIAN_POINT ( 'NONE',  ( -2.620986760973688460E-15, -26.68750000000000000, 13.61880215351699874 ) ) ;
#13566 = ORIENTED_EDGE ( 'NONE', *, *, #16665, .F. ) ;
#13565 = CARTESIAN_POINT ( 'NONE',  ( 1.859271017917182139E-15, 29.33124999877096428, 12.99999999999999289 ) ) ;
#13567 = CARTESIAN_POINT ( 'NONE',  ( 0.000000000000000000, 0.000000000000000000, 17.69999999999999929 ) ) ;
#13568 = DIRECTION ( 'NONE',  ( 1.000000000000000000, 0.000000000000000000, 0.000000000000000000 ) ) ;
#13569 = CARTESIAN_POINT ( 'NONE',  ( -6.741346781237239405, 25.16843286583313954, 20.00001200000000168 ) ) ;
#13570 = CARTESIAN_POINT ( 'NONE',  ( 1.878215178124998497, -29.49062499938548498, 12.25316411605951927 ) ) ;
#13571 = ORIENTED_EDGE ( 'NONE', *, *, #17860, .F. ) ;
#13572 = ORIENTED_EDGE ( 'NONE', *, *, #19626, .F. ) ;
#13573 = CARTESIAN_POINT ( 'NONE',  ( 1.878215178124995832, -25.40312499938548640, 5.746835883940462963 ) ) ;
#13574 = CARTESIAN_POINT ( 'NONE',  ( 4.006172263299091013E-15, 25.47812499938548925, 13.33755215474602984 ) ) ;
#13575 = EDGE_CURVE ( 'NONE', #13450, #18701, #23381, .T. ) ;
#13576 = CARTESIAN_POINT ( 'NONE',  ( 3.735045420075836212E-15, -4.662447845253954171, 1.153124999385480409 ) ) ;
#13577 = CARTESIAN_POINT ( 'NONE',  ( 3.756430356250002323, -11.16877607737301226, 4.715624999385485516 ) ) ;
#13578 = CARTESIAN_POINT ( 'NONE',  ( 1.071796769724485454, -27.51115380933863719, 12.99999999999999467 ) ) ;
#13579 = CARTESIAN_POINT ( 'NONE',  ( 1.071796769724490561, 28.69240381056766864, 4.999999999999988454 ) ) ;
#13580 = DIRECTION ( 'NONE',  ( 1.000000000000000000, 0.000000000000000000, 0.000000000000000000 ) ) ;
#13581 = CARTESIAN_POINT ( 'NONE',  ( -2.875168806925156861, -29.86250404960532379, 11.79623638833883525 ) ) ;
#13582 = DIRECTION ( 'NONE',  ( -0.4817536741017198754, -0.8763066800438610304, 0.000000000000000000 ) ) ;
#13583 = CARTESIAN_POINT ( 'NONE',  ( 3.469446951953614189E-15, -8.999999999999992895, 18.00000000000000000 ) ) ;
#13584 = CARTESIAN_POINT ( 'NONE',  ( 21.71259759894040187, 16.05574334944795112, 11.30940107675849760 ) ) ;
#13585 = VERTEX_POINT ( 'NONE', #3798 ) ;
#13586 = CARTESIAN_POINT ( 'NONE',  ( -4.000000000000003553, -27.64374999877096784, 8.999999999999992895 ) ) ;
#13587 = CARTESIAN_POINT ( 'NONE',  ( 1.626862140677534194E-14, 27.58750000000000213, 12.99999999999999289 ) ) ;
#13588 =( BOUNDED_CURVE ( )  B_SPLINE_CURVE ( 2, ( #22557, #8440, #6341, #20849, #20319, #2938, #16428, #14335, #14578 ),
 .UNSPECIFIED., .F., .F. ) 
 B_SPLINE_CURVE_WITH_KNOTS ( ( 3, 2, 2, 2, 3 ),
 ( 0.9250000000000000444, 0.9333333333333333481, 0.9499999999999999556, 0.9666666666666666741, 0.9749999999999999778 ),
 .UNSPECIFIED. ) 
 CURVE ( )  GEOMETRIC_REPRESENTATION_ITEM ( )  RATIONAL_B_SPLINE_CURVE ( ( 0.9330127018922194093, 0.9330127018922198534, 1.000000000000000000, 0.8660254037844387076, 1.000000000000000000, 0.8660254037844387076, 1.000000000000000000, 0.9330127018922194093, 0.9330127018922194093 ) ) 
 REPRESENTATION_ITEM ( '' )  );
#13589 = CARTESIAN_POINT ( 'NONE',  ( 3.756430356250002323, 28.36562499938548854, 11.16877607737301226 ) ) ;
#13590 = CARTESIAN_POINT ( 'NONE',  ( 4.000000000000003553, -8.999999999999992895, 2.249999999999998668 ) ) ;
#13591 = CARTESIAN_POINT ( 'NONE',  ( -3.999999999999995559, 26.03124999877097068, 6.690598923241487306 ) ) ;
#13592 = CARTESIAN_POINT ( 'NONE',  ( 3.509827456141323410, 38.91143067427094593, 13.34938134445224911 ) ) ;
#13593 = VERTEX_POINT ( 'NONE', #21849 ) ;
#13594 = CARTESIAN_POINT ( 'NONE',  ( 8.831537335106614961E-15, 27.13750000000000284, 12.99999999999999112 ) ) ;
#13595 = DIRECTION ( 'NONE',  ( 0.000000000000000000, -0.000000000000000000, 1.000000000000000000 ) ) ;
#13597 = ORIENTED_EDGE ( 'NONE', *, *, #11664, .T. ) ;
#13596 = CYLINDRICAL_SURFACE ( 'NONE', #2910, 31.10000000000000142 ) ;
#13598 = ORIENTED_EDGE ( 'NONE', *, *, #5684, .T. ) ;
#13599 = VECTOR ( 'NONE', #18310, 1000.000000000000000 ) ;
#13600 = ORIENTED_EDGE ( 'NONE', *, *, #22898, .T. ) ;
#13602 = EDGE_CURVE ( 'NONE', #12823, #1770, #1334, .T. ) ;
#13601 = ORIENTED_EDGE ( 'NONE', *, *, #15136, .T. ) ;
#13603 = VERTEX_POINT ( 'NONE', #11639 ) ;
#13604 = CARTESIAN_POINT ( 'NONE',  ( 3.959305671612554781E-15, 30.00000000000000355, 12.99999999999999289 ) ) ;
#13605 = CARTESIAN_POINT ( 'NONE',  ( -2.000000000000000888, -28.01874999877096784, 12.46410161513774817 ) ) ;
#13606 = LINE ( 'NONE', #21572, #2667 ) ;
#13607 = EDGE_CURVE ( 'NONE', #8280, #1701, #25763, .T. ) ;
#13608 = AXIS2_PLACEMENT_3D ( 'NONE', #21188, #11240, #23277 ) ;
#13609 = CARTESIAN_POINT ( 'NONE',  ( 3.756430356250003655, -8.999999999999992895, 1.940624999385482496 ) ) ;
#13610 = CARTESIAN_POINT ( 'NONE',  ( 2.000000000000000888, -12.46410161513774817, 3.018749998770966503 ) ) ;
#13611 = CARTESIAN_POINT ( 'NONE',  ( 1.878215178125000939, 28.77812499938548640, 12.25316411605952283 ) ) ;
#13612 = DIRECTION ( 'NONE',  ( 0.000000000000000000, 0.000000000000000000, 1.000000000000000000 ) ) ;
#13613 = CARTESIAN_POINT ( 'NONE',  ( 23.01025686871630782, -20.92219106202058754, -6.500000000000000000 ) ) ;
#13614 = CARTESIAN_POINT ( 'NONE',  ( -3.999999999999996003, -6.690598923241487306, 2.887499999999999289 ) ) ;
#13615 =( REPRESENTATION_RELATIONSHIP ('NONE','NONE', #25031, #23343 ) REPRESENTATION_RELATIONSHIP_WITH_TRANSFORMATION ( #12192 )SHAPE_REPRESENTATION_RELATIONSHIP( ) );
#13616 = DIRECTION ( 'NONE',  ( 0.000000000000000000, 0.000000000000000000, -1.000000000000000000 ) ) ;
#13617 = LINE ( 'NONE', #13497, #22476 ) ;
#13618 = CARTESIAN_POINT ( 'NONE',  ( 3.469446951953614189E-15, 40.00000000000000000, 8.999999999999992895 ) ) ;
#13619 = CARTESIAN_POINT ( 'NONE',  ( -4.000000000000001776, -26.25624999877096499, 11.30940107675849760 ) ) ;
#13620 = CARTESIAN_POINT ( 'NONE',  ( 2.672651547586948120E-15, 27.39062499938548356, 13.33755215474602984 ) ) ;
#13621 = DIRECTION ( 'NONE',  ( 0.000000000000000000, 0.000000000000000000, 1.000000000000000000 ) ) ;
#13622 = LINE ( 'NONE', #21589, #1197 ) ;
#13623 = LINE ( 'NONE', #7607, #18086 ) ;
#13624 = ORIENTED_EDGE ( 'NONE', *, *, #8861, .F. ) ;
#13625 = CYLINDRICAL_SURFACE ( 'NONE', #5424, 0.5000000000000004441 ) ;
#13626 = ORIENTED_EDGE ( 'NONE', *, *, #4873, .F. ) ;
#13627 = ORIENTED_EDGE ( 'NONE', *, *, #24388, .T. ) ;
#13628 = CARTESIAN_POINT ( 'NONE',  ( -19.32388608118446527, -23.96296185032687376, -6.500000000000000000 ) ) ;
#13629 = ORIENTED_EDGE ( 'NONE', *, *, #3429, .F. ) ;
#13630 = CARTESIAN_POINT ( 'NONE',  ( 1.878215178124995832, -27.65312499938548640, 5.746835883940462963 ) ) ;
#13631 = ORIENTED_EDGE ( 'NONE', *, *, #15566, .F. ) ;
#13632 = CARTESIAN_POINT ( 'NONE',  ( -4.393401135980685268, 30.78811501957149588, -6.500000000000000000 ) ) ;
#13633 = EDGE_CURVE ( 'NONE', #11588, #6934, #18794, .T. ) ;
#13634 = ORIENTED_EDGE ( 'NONE', *, *, #2638, .T. ) ;
#13635 = EDGE_CURVE ( 'NONE', #22996, #11790, #3413, .T. ) ;
#13636 = CARTESIAN_POINT ( 'NONE',  ( 4.000000000000003553, 27.28749999999999787, 6.690598923241489970 ) ) ;
#13637 = CARTESIAN_POINT ( 'NONE',  ( 3.469446951953614189E-15, 40.00000000000000000, 4.999999999999992006 ) ) ;
#13638 = CARTESIAN_POINT ( 'NONE',  ( 31.06601413805602618, 1.453535542772499856, -6.500000000000000000 ) ) ;
#13639 = CARTESIAN_POINT ( 'NONE',  ( -30.54913349766215802, 5.827558883616378083, 1.000000000000000000 ) ) ;
#13640 = CARTESIAN_POINT ( 'NONE',  ( 17.85665593321704137, 17.85665593321697742, 4.662447845253954171 ) ) ;
#13641 = EDGE_CURVE ( 'NONE', #25152, #24761, #2930, .T. ) ;
#13642 = DIRECTION ( 'NONE',  ( 0.000000000000000000, 0.000000000000000000, 1.000000000000000000 ) ) ;
#13643 = CARTESIAN_POINT ( 'NONE',  ( 2.000000000000000888, 28.07500000000000284, 12.46410161513774817 ) ) ;
#13644 = CARTESIAN_POINT ( 'NONE',  ( 3.469446951953614189E-15, 39.50000000000000000, 8.999999999999992895 ) ) ;
#13645 = DIRECTION ( 'NONE',  ( 0.000000000000000000, 0.000000000000000000, 1.000000000000000000 ) ) ;
#13646 = CARTESIAN_POINT ( 'NONE',  ( 4.000000000000000888, 28.11250000000000071, 11.30940107675849760 ) ) ;
#13647 = VERTEX_POINT ( 'NONE', #23802 ) ;
#13648 = ORIENTED_EDGE ( 'NONE', *, *, #4012, .F. ) ;
#13649 = CARTESIAN_POINT ( 'NONE',  ( 4.000000000000002665, 29.40624999877096357, 11.30940107675849760 ) ) ;
#13650 = ORIENTED_EDGE ( 'NONE', *, *, #5915, .T. ) ;
#13651 = DIRECTION ( 'NONE',  ( 0.000000000000000000, 1.000000000000000000, 0.000000000000000000 ) ) ;
#13652 = CARTESIAN_POINT ( 'NONE',  ( -3.756430356249997882, 29.56562499938549138, 11.16877607737301226 ) ) ;
#13653 = CARTESIAN_POINT ( 'NONE',  ( 1.453535542772391942, -31.06601413805603329, -6.500000000000000000 ) ) ;
#13654 = ORIENTED_EDGE ( 'NONE', *, *, #17402, .T. ) ;
#13655 = ORIENTED_EDGE ( 'NONE', *, *, #13421, .T. ) ;
#13656 = CARTESIAN_POINT ( 'NONE',  ( 31.09598070739550479, 0.4999838450258676792, -2.750000000000000000 ) ) ;
#13657 = ORIENTED_EDGE ( 'NONE', *, *, #1724, .T. ) ;
#13658 = DIRECTION ( 'NONE',  ( 0.000000000000000000, 1.000000000000000000, 0.000000000000000000 ) ) ;
#13659 = CARTESIAN_POINT ( 'NONE',  ( -24.66042852506064165, 18.28012134629622309, 1.000000000000000000 ) ) ;
#13660 = CARTESIAN_POINT ( 'NONE',  ( 2.003086131649545506E-15, 29.07812499938549067, 13.33755215474603162 ) ) ;
#13661 = DIRECTION ( 'NONE',  ( 0.000000000000000000, 0.000000000000000000, -1.000000000000000000 ) ) ;
#13662 = CARTESIAN_POINT ( 'NONE',  ( -3.999999999999996447, 27.92500000000000426, 8.999999999999992895 ) ) ;
#13663 = ADVANCED_FACE ( 'NONE', ( #9309 ), #17294, .F. ) ;
#13664 = EDGE_CURVE ( 'NONE', #5148, #15562, #11280, .T. ) ;
#13665 = CARTESIAN_POINT ( 'NONE',  ( -3.756430356249995661, 25.32812499938548356, 6.831223922626973533 ) ) ;
#13666 = CARTESIAN_POINT ( 'NONE',  ( 26.49999999999999645, 0.5000000000000000000, 19.00000000000000000 ) ) ;
#13667 = EDGE_CURVE ( 'NONE', #5989, #6393, #12537, .T. ) ;
#13668 = CARTESIAN_POINT ( 'NONE',  ( -20.78941499438192508, 22.67092431280617859, -6.500000000000000000 ) ) ;
#13669 = CARTESIAN_POINT ( 'NONE',  ( -1.042539689874651954, -29.98299368898127071, 5.129272290912049392 ) ) ;
#13670 = CARTESIAN_POINT ( 'NONE',  ( 19.34820930021694352, 19.34820930021687246, 4.381197846482986158 ) ) ;
#13671 = CARTESIAN_POINT ( 'NONE',  ( 21.99550407741325486, 19.33930669945380743, 12.25316411605952283 ) ) ;
#13672 = CARTESIAN_POINT ( 'NONE',  ( -4.000000000000057732, -6.690598923241522833, 4.631249998770965881 ) ) ;
#13673 = CARTESIAN_POINT ( 'NONE',  ( 3.756430356250002323, 29.15312499938548640, 11.16877607737301226 ) ) ;
#13674 = CARTESIAN_POINT ( 'NONE',  ( 4.000000000000000888, 27.15624999877097423, 11.30940107675849760 ) ) ;
#13675 = DIRECTION ( 'NONE',  ( 0.000000000000000000, 0.000000000000000000, -1.000000000000000000 ) ) ;
#13676 = CARTESIAN_POINT ( 'NONE',  ( 4.393401135980900207, -30.78811501957146390, -2.750000000000000000 ) ) ;
#13677 = ORIENTED_EDGE ( 'NONE', *, *, #24315, .T. ) ;
#13678 = CARTESIAN_POINT ( 'NONE',  ( 4.000000000000001776, 26.25624999877096499, 11.30940107675849760 ) ) ;
#13679 = CARTESIAN_POINT ( 'NONE',  ( -3.752267015613588906E-15, -26.46250000000000213, 4.381197846482986158 ) ) ;
#13681 = ORIENTED_EDGE ( 'NONE', *, *, #782, .T. ) ;
#13680 = CARTESIAN_POINT ( 'NONE',  ( 1.878215178125005158, 25.77812499938548996, 5.746835883940462963 ) ) ;
#13682 = CARTESIAN_POINT ( 'NONE',  ( 3.756430356250003211, 28.44062499938548427, 6.831223922626973533 ) ) ;
#13683 = DIRECTION ( 'NONE',  ( 0.000000000000000000, 0.000000000000000000, 1.000000000000000000 ) ) ;
#13684 = ORIENTED_EDGE ( 'NONE', *, *, #18697, .T. ) ;
#13685 = DIRECTION ( 'NONE',  ( 0.000000000000000000, 0.000000000000000000, 1.000000000000000000 ) ) ;
#13686 = VERTEX_POINT ( 'NONE', #23554 ) ;
#13687 = ORIENTED_EDGE ( 'NONE', *, *, #6708, .F. ) ;
#13688 = DIRECTION ( 'NONE',  ( 0.000000000000000000, 0.000000000000000000, 1.000000000000000000 ) ) ;
#13689 = CARTESIAN_POINT ( 'NONE',  ( 3.756430356250004543, 26.07812499938549422, 6.831223922626973533 ) ) ;
#13690 = EDGE_CURVE ( 'NONE', #10718, #21413, #3331, .T. ) ;
#13691 = CARTESIAN_POINT ( 'NONE',  ( 3.756430356250003211, -6.831223922626973533, 2.428124999385481431 ) ) ;
#13692 = ADVANCED_FACE ( 'NONE', ( #24326 ), #24059, .F. ) ;
#13693 = AXIS2_PLACEMENT_3D ( 'NONE', #9050, #23292, #22914 ) ;
#13694 = CARTESIAN_POINT ( 'NONE',  ( 0.5000000000000000000, 6.000000000000000000, 20.00000000000000000 ) ) ;
#13695 = SHAPE_REPRESENTATION_RELATIONSHIP ( 'NONE' , 'NONE' ,  #22515, #4445 ) ;
#13696 = CARTESIAN_POINT ( 'NONE',  ( 30.91344420362548107, 3.401318489840985837, -6.500000000000000000 ) ) ;
#13697 = CARTESIAN_POINT ( 'NONE',  ( -29.09636799667091367, -10.98232076577190774, -2.750000000000000000 ) ) ;
#13698 = CARTESIAN_POINT ( 'NONE',  ( 30.45149776762727356, -6.317933499823421784, 1.000000000000000000 ) ) ;
#13699 = FACE_OUTER_BOUND ( 'NONE', #16137, .T. ) ;
#13700 = CARTESIAN_POINT ( 'NONE',  ( -3.469446951953614189E-15, -30.00000000000000355, 8.999999999999992895 ) ) ;
#13701 = CARTESIAN_POINT ( 'NONE',  ( -16.23990935651690748, 26.52310962334761157, 1.000000000000000000 ) ) ;
#13702 = CARTESIAN_POINT ( 'NONE',  ( 20.81103645292755289, 15.15418220343510392, 6.690598923241489970 ) ) ;
#13703 = VERTEX_POINT ( 'NONE', #6142 ) ;
#13704 = CARTESIAN_POINT ( 'NONE',  ( -3.999999999999997335, 27.51250000000000284, 11.30940107675849404 ) ) ;
#13705 = CARTESIAN_POINT ( 'NONE',  ( 3.756430356249996994, -29.07812499938548356, 8.999999999999992895 ) ) ;
#13706 = CARTESIAN_POINT ( 'NONE',  ( 3.756430356250003655, 28.85312499938548569, 8.999999999999992895 ) ) ;
#13707 = EDGE_CURVE ( 'NONE', #7429, #1277, #22091, .T. ) ;
#13708 = DIRECTION ( 'NONE',  ( 0.000000000000000000, 0.000000000000000000, 1.000000000000000000 ) ) ;
#13709 = CARTESIAN_POINT ( 'NONE',  ( 4.000000000000003553, 29.03124999877096712, 6.690598923241489970 ) ) ;
#13710 = ORIENTED_EDGE ( 'NONE', *, *, #12336, .T. ) ;
#13711 = CARTESIAN_POINT ( 'NONE',  ( 2.620986760973688460E-15, -13.61880215351699874, 2.587499999999999467 ) ) ;
#13712 = CARTESIAN_POINT ( 'NONE',  ( -5.532151103383257329, 38.49999999999999289, 6.677220593914388935 ) ) ;
#13714 = ORIENTED_EDGE ( 'NONE', *, *, #7238, .F. ) ;
#13713 = DIRECTION ( 'NONE',  ( 1.000000000000000000, 0.000000000000000000, 0.000000000000000000 ) ) ;
#13715 = ORIENTED_EDGE ( 'NONE', *, *, #21059, .T. ) ;
#13716 = ORIENTED_EDGE ( 'NONE', *, *, #9465, .T. ) ;
#13717 = VERTEX_POINT ( 'NONE', #12292 ) ;
#13718 = ORIENTED_EDGE ( 'NONE', *, *, #23187, .T. ) ;
#13719 = CARTESIAN_POINT ( 'NONE',  ( 0.000000000000000000, 0.000000000000000000, -6.500000000000000000 ) ) ;
#13720 = CARTESIAN_POINT ( 'NONE',  ( -3.369773278825879181, 38.97868814324865383, 13.37417080150618354 ) ) ;
#13721 = AXIS2_PLACEMENT_3D ( 'NONE', #12988, #11017, #12850 ) ;
#13722 = VECTOR ( 'NONE', #17264, 1000.000000000000000 ) ;
#13723 = CYLINDRICAL_SURFACE ( 'NONE', #973, 0.7500000000000001110 ) ;
#13724 = DIRECTION ( 'NONE',  ( 0.000000000000000000, 0.000000000000000000, 1.000000000000000000 ) ) ;
#13725 = CARTESIAN_POINT ( 'NONE',  ( -1.878215178124995832, -5.746835883940462963, 2.090624999385483296 ) ) ;
#13726 = CARTESIAN_POINT ( 'NONE',  ( -3.756430356249995661, -6.831223922626973533, 0.4406249993854817193 ) ) ;
#13727 =( NAMED_UNIT ( * ) PLANE_ANGLE_UNIT ( ) SI_UNIT ( $, .RADIAN. ) );
#13728 = B_SPLINE_CURVE_WITH_KNOTS ( 'NONE', 3,
 ( #21554, #3381, #5343, #5607 ),
 .UNSPECIFIED., .F., .F.,
 ( 4, 4 ),
 ( 0.001666568017356004870, 0.001856323057641126682 ),
 .UNSPECIFIED. ) ;
#13729 =( BOUNDED_CURVE ( )  B_SPLINE_CURVE ( 2, ( #16551, #6592, #12229, #6081, #14066, #22032, #210, #8180, #4254 ),
 .UNSPECIFIED., .F., .F. ) 
 B_SPLINE_CURVE_WITH_KNOTS ( ( 3, 2, 2, 2, 3 ),
 ( 0.6750000000000000444, 0.6833333333333333481, 0.6999999999999999556, 0.7166666666666666741, 0.7249999999999999778 ),
 .UNSPECIFIED. ) 
 CURVE ( )  GEOMETRIC_REPRESENTATION_ITEM ( )  RATIONAL_B_SPLINE_CURVE ( ( 0.9330127018922194093, 0.9330127018922198534, 1.000000000000000000, 0.8660254037844387076, 1.000000000000000000, 0.8660254037844387076, 1.000000000000000000, 0.9330127018922194093, 0.9330127018922194093 ) ) 
 REPRESENTATION_ITEM ( '' )  );
#13730 = CARTESIAN_POINT ( 'NONE',  ( -1.878215178124995832, 28.55312499938548498, 5.746835883940462963 ) ) ;
#13731 = ADVANCED_FACE ( 'NONE', ( #14002 ), #2098, .F. ) ;
#13732 = LINE ( 'NONE', #23551, #10857 ) ;
#13733 = AXIS2_PLACEMENT_3D ( 'NONE', #16041, #14067, #4501 ) ;
#13734 = DIRECTION ( 'NONE',  ( 0.000000000000000000, 0.000000000000000000, 1.000000000000000000 ) ) ;
#13735 = CARTESIAN_POINT ( 'NONE',  ( 2.000000000000003997, -5.535898384862238508, 0.9750000000000001998 ) ) ;
#13736 = VECTOR ( 'NONE', #1910, 999.9999999999998863 ) ;
#13737 = CARTESIAN_POINT ( 'NONE',  ( 0.000000000000000000, 0.000000000000000000, 1.000000000000000000 ) ) ;
#13738 = CARTESIAN_POINT ( 'NONE',  ( 2.620986760973688460E-15, -13.61880215351699874, 2.531249998770966236 ) ) ;
#13739 = DIRECTION ( 'NONE',  ( 0.000000000000000000, 0.000000000000000000, 1.000000000000000000 ) ) ;
#13740 = CARTESIAN_POINT ( 'NONE',  ( -3.752267015613588906E-15, -27.30624999877097281, 4.381197846482986158 ) ) ;
#13741 = CARTESIAN_POINT ( 'NONE',  ( -3.756430356249995661, 29.04062499938548569, 6.831223922626973533 ) ) ;
#13742 = VECTOR ( 'NONE', #17068, 1000.000000000000000 ) ;
#13743 = DIRECTION ( 'NONE',  ( 1.000000000000000000, 0.000000000000000000, -0.000000000000000000 ) ) ;
#13745 = CARTESIAN_POINT ( 'NONE',  ( 2.000000000000000000, 28.01874999877097139, 12.46410161513774817 ) ) ;
#13744 = AXIS2_PLACEMENT_3D ( 'NONE', #19205, #21307, #9285 ) ;
#13746 = CARTESIAN_POINT ( 'NONE',  ( 1.999999999999995781, -25.99374999877096926, 5.535898384862237620 ) ) ;
#13747 = ORIENTED_EDGE ( 'NONE', *, *, #18103, .T. ) ;
#13748 = ORIENTED_EDGE ( 'NONE', *, *, #7657, .F. ) ;
#13749 = ORIENTED_EDGE ( 'NONE', *, *, #5336, .F. ) ;
#13750 = DIRECTION ( 'NONE',  ( 0.000000000000000000, 0.000000000000000000, -1.000000000000000000 ) ) ;
#13751 = ORIENTED_EDGE ( 'NONE', *, *, #20794, .T. ) ;
#13752 = CARTESIAN_POINT ( 'NONE',  ( 1.878215178124995832, -28.55312499938548498, 5.746835883940462963 ) ) ;
#13753 = ORIENTED_EDGE ( 'NONE', *, *, #5206, .T. ) ;
#13754 = DIRECTION ( 'NONE',  ( 1.000000000000000000, 0.000000000000000000, 0.000000000000000000 ) ) ;
#13755 = AXIS2_PLACEMENT_3D ( 'NONE', #15687, #11882, #1831 ) ;
#13756 = ORIENTED_EDGE ( 'NONE', *, *, #7074, .T. ) ;
#13757 = CARTESIAN_POINT ( 'NONE',  ( 2.000000000000000888, 26.72500000000000142, 12.46410161513774817 ) ) ;
#13758 = CARTESIAN_POINT ( 'NONE',  ( 0.000000000000000000, 0.000000000000000000, 20.00000000000000000 ) ) ;
#13759 = CIRCLE ( 'NONE', #20429, 0.5000000000000005551 ) ;
#13760 = CIRCLE ( 'NONE', #12500, 0.7500000000000001110 ) ;
#13761 = CYLINDRICAL_SURFACE ( 'NONE', #7982, 0.5000000000000004441 ) ;
#13762 = CARTESIAN_POINT ( 'NONE',  ( -2.999999999999996891, -8.999999999999992895, 0.000000000000000000 ) ) ;
#13763 = CARTESIAN_POINT ( 'NONE',  ( 17.58694394176227149, 22.89933869768094610, 8.999999999999992895 ) ) ;
#13764 = CARTESIAN_POINT ( 'NONE',  ( -1.999999999999993117, 27.34374999877097068, 5.535898384862237620 ) ) ;
#13765 = ADVANCED_FACE ( 'NONE', ( #6021 ), #14126, .T. ) ;
#13766 = DIRECTION ( 'NONE',  ( -0.000000000000000000, -1.000000000000000000, -0.000000000000000000 ) ) ;
#13768 = AXIS2_PLACEMENT_3D ( 'NONE', #6539, #16371, #24336 ) ;
#13767 = APPLICATION_PROTOCOL_DEFINITION ( 'draft international standard', 'automotive_design', 1998, #13960 ) ;
#13769 = CARTESIAN_POINT ( 'NONE',  ( 4.000000000000003553, 29.05000000000000071, 8.999999999999992895 ) ) ;
#13770 = AXIS2_PLACEMENT_3D ( 'NONE', #8203, #6232, #4140 ) ;
#13771 = CARTESIAN_POINT ( 'NONE',  ( -1.878215178124998497, -12.25316411605951927, 0.5531249993854860936 ) ) ;
#13772 = EDGE_CURVE ( 'NONE', #4937, #8646, #15974, .T. ) ;
#13773 = CARTESIAN_POINT ( 'NONE',  ( -6.317933499823659815, -30.45149776762723093, -2.750000000000000000 ) ) ;
#13774 = DIRECTION ( 'NONE',  ( -0.000000000000000000, -0.000000000000000000, 1.000000000000000000 ) ) ;
#13775 = AXIS2_PLACEMENT_3D ( 'NONE', #14759, #16715, #22858 ) ;
#13776 = VERTEX_POINT ( 'NONE', #12158 ) ;
#13778 = ADVANCED_FACE ( 'NONE', ( #23938 ), #21974, .F. ) ;
#13777 = ORIENTED_EDGE ( 'NONE', *, *, #5528, .F. ) ;
#13779 = CARTESIAN_POINT ( 'NONE',  ( 4.000000000000002665, 29.03124999877097423, 6.690598923241489970 ) ) ;
#13780 = ORIENTED_EDGE ( 'NONE', *, *, #6590, .F. ) ;
#13781 = CARTESIAN_POINT ( 'NONE',  ( -3.999999999999995559, 26.03124999877097068, 6.690598923241487306 ) ) ;
#13782 = CIRCLE ( 'NONE', #21243, 31.10000000000000142 ) ;
#13783 = LINE ( 'NONE', #21760, #920 ) ;
#13784 = CARTESIAN_POINT ( 'NONE',  ( 0.000000000000000000, 0.000000000000000000, -6.500000000000000000 ) ) ;
#13785 = EDGE_CURVE ( 'NONE', #11788, #19594, #39, .T. ) ;
#13786 = ORIENTED_EDGE ( 'NONE', *, *, #25003, .T. ) ;
#13787 = VERTEX_POINT ( 'NONE', #11900 ) ;
#13788 = DIRECTION ( 'NONE',  ( 0.6845471059286972748, 0.7289686274214034478, 0.000000000000000000 ) ) ;
#13789 = AXIS2_PLACEMENT_3D ( 'NONE', #7961, #2076, #15947 ) ;
#13790 = ORIENTED_EDGE ( 'NONE', *, *, #19445, .F. ) ;
#13791 = CARTESIAN_POINT ( 'NONE',  ( 0.4860084296119324132, 38.61007524145222192, 14.86986133562586865 ) ) ;
#13792 = DIRECTION ( 'NONE',  ( 0.000000000000000000, 0.000000000000000000, 1.000000000000000000 ) ) ;
#13793 = CARTESIAN_POINT ( 'NONE',  ( 3.756430356250003211, 27.39062499938548711, 8.999999999999992895 ) ) ;
#13794 = VECTOR ( 'NONE', #17539, 1000.000000000000000 ) ;
#13795 = CIRCLE ( 'NONE', #17569, 0.5000000000000003331 ) ;
#13796 = CARTESIAN_POINT ( 'NONE',  ( -4.000000000000003553, -26.83749999999999503, 6.690598923241489970 ) ) ;
#13797 = CARTESIAN_POINT ( 'NONE',  ( -1.999999999999994893, 26.05000000000000426, 5.535898384862237620 ) ) ;
#13798 = CIRCLE ( 'NONE', #6699, 31.10000000000000142 ) ;
#13799 = CARTESIAN_POINT ( 'NONE',  ( 18.28012134629595309, 25.16042852506084770, 1.000000000000000000 ) ) ;
#13800 = CARTESIAN_POINT ( 'NONE',  ( 20.46190248058575634, 20.46190248058568173, 12.99999999999999289 ) ) ;
#13801 = CARTESIAN_POINT ( 'NONE',  ( -24.66042852506104310, -18.28012134629567598, -6.500000000000000000 ) ) ;
#13802 = CARTESIAN_POINT ( 'NONE',  ( 21.26623644418545211, 18.43780931943919299, 12.46410161513774817 ) ) ;
#13803 = CARTESIAN_POINT ( 'NONE',  ( 20.16359180683815921, 20.16359180683807750, 4.662447845253954171 ) ) ;
#13804 = EDGE_CURVE ( 'NONE', #13187, #14350, #2948, .T. ) ;
#13805 = DIRECTION ( 'NONE',  ( 0.000000000000000000, 0.000000000000000000, 1.000000000000000000 ) ) ;
#13806 = CARTESIAN_POINT ( 'NONE',  ( 2.000000000000003997, 28.22500000000000142, 5.535898384862238508 ) ) ;
#13807 = AXIS2_PLACEMENT_3D ( 'NONE', #22354, #8120, #19994 ) ;
#13808 = DIRECTION ( 'NONE',  ( -0.7071067811865487940, -0.7071067811865463515, 0.000000000000000000 ) ) ;
#13809 = AXIS2_PLACEMENT_3D ( 'NONE', #9581, #25544, #1993 ) ;
#13810 = CARTESIAN_POINT ( 'NONE',  ( 22.23415261606371374, 19.57795523810426630, 12.25316411605952283 ) ) ;
#13811 = CARTESIAN_POINT ( 'NONE',  ( -12.78762572734076919, -28.34936733434192035, -6.500000000000000000 ) ) ;
#13812 = ORIENTED_EDGE ( 'NONE', *, *, #19418, .F. ) ;
#13813 = CARTESIAN_POINT ( 'NONE',  ( 2.000000000000003997, 26.81874999877096855, 5.535898384862238508 ) ) ;
#13814 = CARTESIAN_POINT ( 'NONE',  ( 1.999999999999998224, -27.10000000000000142, 12.46410161513774639 ) ) ;
#13815 = EDGE_CURVE ( 'NONE', #10117, #3578, #16729, .T. ) ;
#13817 = ORIENTED_EDGE ( 'NONE', *, *, #4215, .T. ) ;
#13816 = CARTESIAN_POINT ( 'NONE',  ( 3.756430356250003211, 26.15312499938548996, 8.999999999999992895 ) ) ;
#13818 = CARTESIAN_POINT ( 'NONE',  ( -3.756430356249996105, 29.49062499938548498, 6.831223922626973533 ) ) ;
#13820 = ADVANCED_FACE ( 'NONE', ( #19868 ), #16095, .F. ) ;
#13819 = AXIS2_PLACEMENT_3D ( 'NONE', #15970, #18063, #7841 ) ;
#13821 = CARTESIAN_POINT ( 'NONE',  ( 1.999999999999995781, -29.59374999877096712, 5.535898384862237620 ) ) ;
#13822 = CARTESIAN_POINT ( 'NONE',  ( 20.67279826512042007, 15.85973458909327860, 20.00001200000000523 ) ) ;
#13823 = LINE ( 'NONE', #5972, #25510 ) ;
#13824 = EDGE_LOOP ( 'NONE', ( #6006, #7371, #16758, #24976 ) ) ;
#13825 = ORIENTED_EDGE ( 'NONE', *, *, #24499, .T. ) ;
#13826 =( NAMED_UNIT ( * ) SI_UNIT ( $, .STERADIAN. ) SOLID_ANGLE_UNIT ( ) );
#13827 = CARTESIAN_POINT ( 'NONE',  ( -3.756430356249998326, 29.04062499938548569, 6.831223922626973533 ) ) ;
#13828 = CARTESIAN_POINT ( 'NONE',  ( 3.756430356250003655, -8.999999999999992895, 4.190624999385480720 ) ) ;
#13829 = AXIS2_PLACEMENT_3D ( 'NONE', #18792, #12782, #2832 ) ;
#13830 = VECTOR ( 'NONE', #14743, 1000.000000000000000 ) ;
#13831 = CARTESIAN_POINT ( 'NONE',  ( -1.071796769724490117, 27.32634618820330630, 4.999999999999992895 ) ) ;
#13832 =( NAMED_UNIT ( * ) SI_UNIT ( $, .STERADIAN. ) SOLID_ANGLE_UNIT ( ) );
#13833 = CARTESIAN_POINT ( 'NONE',  ( 6.938893903907228378E-15, 31.50000000000000000, 2.999999999999992450 ) ) ;
#13834 = DIRECTION ( 'NONE',  ( 0.000000000000000000, 0.000000000000000000, 1.000000000000000000 ) ) ;
#13835 = DIRECTION ( 'NONE',  ( 0.000000000000000000, 0.000000000000000000, 1.000000000000000000 ) ) ;
#13836 = LINE ( 'NONE', #5852, #12895 ) ;
#13837 = DIRECTION ( 'NONE',  ( -1.000000000000000000, 0.000000000000000000, 0.000000000000000000 ) ) ;
#13838 = CARTESIAN_POINT ( 'NONE',  ( 16.87327180006579752, 19.52946917802510285, 5.746835883940462963 ) ) ;
#13839 = CARTESIAN_POINT ( 'NONE',  ( -3.469446951953614189E-15, -30.00000000000000355, 4.999999999999992006 ) ) ;
#13840 = EDGE_LOOP ( 'NONE', ( #13857, #12956, #4161, #21695 ) ) ;
#13841 = CARTESIAN_POINT ( 'NONE',  ( -5.450524252594506791, 38.86762122992237067, 10.42016860233466247 ) ) ;
#13842 = CARTESIAN_POINT ( 'NONE',  ( 2.007320019195686811, 29.93357098804190741, 5.530155478426868498 ) ) ;
#13843 = CARTESIAN_POINT ( 'NONE',  ( -3.756430356249996994, 27.72812499938548569, 8.999999999999992895 ) ) ;
#13844 = CARTESIAN_POINT ( 'NONE',  ( -11.44867358849309547, 28.91604871112477326, -6.500000000000000000 ) ) ;
#13845 = AXIS2_PLACEMENT_3D ( 'NONE', #5775, #12043, #11803 ) ;
#13846 = EDGE_CURVE ( 'NONE', #2002, #5285, #23830, .T. ) ;
#13847 = CARTESIAN_POINT ( 'NONE',  ( 3.694956938997175477, 38.77026726007181878, 13.37932843446066045 ) ) ;
#13848 = VERTEX_POINT ( 'NONE', #12411 ) ;
#13849 = CARTESIAN_POINT ( 'NONE',  ( 1.999999999999998224, 26.66874999877097352, 12.46410161513774817 ) ) ;
#13850 = CARTESIAN_POINT ( 'NONE',  ( 31.03863125411924173, -1.952785157361756951, -6.500000000000000000 ) ) ;
#13852 = VERTEX_POINT ( 'NONE', #24451 ) ;
#13851 = DIRECTION ( 'NONE',  ( -1.000000000000000000, 0.000000000000000000, 0.000000000000000000 ) ) ;
#13853 = VECTOR ( 'NONE', #15299, 1000.000000000000000 ) ;
#13854 = EDGE_CURVE ( 'NONE', #10597, #2759, #11300, .T. ) ;
#13855 = VECTOR ( 'NONE', #11700, 1000.000000000000000 ) ;
#13856 = EDGE_LOOP ( 'NONE', ( #25418, #17554, #23441, #18388 ) ) ;
#13857 = ORIENTED_EDGE ( 'NONE', *, *, #14297, .F. ) ;
#13858 = EDGE_LOOP ( 'NONE', ( #1742, #11554, #24030, #12957 ) ) ;
#13859 = VERTEX_POINT ( 'NONE', #24186 ) ;
#13860 = CARTESIAN_POINT ( 'NONE',  ( 7.437084071668728555E-15, 27.13750000000000639, 12.99999999999999112 ) ) ;
#13862 = FACE_BOUND ( 'NONE', #3187, .T. ) ;
#13861 = AXIS2_PLACEMENT_3D ( 'NONE', #7658, #7908, #15895 ) ;
#13863 = PRESENTATION_STYLE_ASSIGNMENT (( #13991 ) ) ;
#13864 = CARTESIAN_POINT ( 'NONE',  ( -3.756430356249996105, 27.65312499938548996, 11.16877607737301226 ) ) ;
#13865 = AXIS2_PLACEMENT_3D ( 'NONE', #3824, #19641, #15611 ) ;
#13866 = CARTESIAN_POINT ( 'NONE',  ( 3.735045420075836212E-15, -4.662447845253954171, 3.853124999385482585 ) ) ;
#13867 = CARTESIAN_POINT ( 'NONE',  ( 4.000000000000003553, -6.690598923241489970, 4.031249998770966236 ) ) ;
#13868 = AXIS2_PLACEMENT_3D ( 'NONE', #18186, #20256, #10308 ) ;
#13869 = CARTESIAN_POINT ( 'NONE',  ( 3.735045420075836212E-15, 29.41562499938548569, 4.662447845253954171 ) ) ;
#13870 = CIRCLE ( 'NONE', #24322, 31.10000000000000142 ) ;
#13871 = DIRECTION ( 'NONE',  ( 0.000000000000000000, -0.000000000000000000, 1.000000000000000000 ) ) ;
#13872 = CYLINDRICAL_SURFACE ( 'NONE', #5931, 0.5000000000000004441 ) ;
#13873 = CARTESIAN_POINT ( 'NONE',  ( -3.999999999999997335, -11.30940107675849404, 2.062499999999998224 ) ) ;
#13874 = AXIS2_PLACEMENT_3D ( 'NONE', #25308, #13792, #7649 ) ;
#13875 = CARTESIAN_POINT ( 'NONE',  ( -7.734255490826573265, 30.12293631110053838, -6.500000000000000000 ) ) ;
#13876 = PLANE ( 'NONE',  #9106 ) ;
#13877 = CARTESIAN_POINT ( 'NONE',  ( -0.5000000000000001110, 0.000000000000000000, 19.50000000000000000 ) ) ;
#13878 = CARTESIAN_POINT ( 'NONE',  ( -2.000000000000003997, -29.51874999877096784, 5.535898384862238508 ) ) ;
#13879 = AXIS2_PLACEMENT_3D ( 'NONE', #24412, #6607, #12373 ) ;
#13880 = CARTESIAN_POINT ( 'NONE',  ( -1.878215178124998497, 27.35312499938548569, 12.25316411605951927 ) ) ;
#13881 = CARTESIAN_POINT ( 'NONE',  ( -7.734255490827218971, -30.12293631110037140, 1.000000000000000000 ) ) ;
#13882 = DIRECTION ( 'NONE',  ( 0.7071067811865487940, 0.7071067811865463515, 0.000000000000000000 ) ) ;
#13883 = PLANE ( 'NONE',  #121 ) ;
#13884 = ORIENTED_EDGE ( 'NONE', *, *, #10895, .F. ) ;
#13885 = LINE ( 'NONE', #1978, #16276 ) ;
#13887 = ORIENTED_EDGE ( 'NONE', *, *, #13106, .F. ) ;
#13886 = CARTESIAN_POINT ( 'NONE',  ( 2.000000000000003997, 28.22500000000000142, 5.535898384862238508 ) ) ;
#13888 = EDGE_CURVE ( 'NONE', #19523, #25423, #6275, .T. ) ;
#13889 = AXIS2_PLACEMENT_3D ( 'NONE', #20398, #14798, #24346 ) ;
#13890 = VERTEX_POINT ( 'NONE', #18305 ) ;
#13891 = DIRECTION ( 'NONE',  ( 0.000000000000000000, 0.000000000000000000, 1.000000000000000000 ) ) ;
#13892 = VERTEX_POINT ( 'NONE', #398 ) ;
#13893 = CARTESIAN_POINT ( 'NONE',  ( -1.878215178125000939, -26.41562499938548214, 12.25316411605952283 ) ) ;
#13894 = ORIENTED_EDGE ( 'NONE', *, *, #11086, .F. ) ;
#13895 = DIRECTION ( 'NONE',  ( -0.000000000000000000, -1.000000000000000000, -0.000000000000000000 ) ) ;
#13896 = ADVANCED_FACE ( 'NONE', ( #10446 ), #9933, .T. ) ;
#13897 = CIRCLE ( 'NONE', #4709, 1.000000000000000000 ) ;
#13898 = ORIENTED_EDGE ( 'NONE', *, *, #9394, .F. ) ;
#13899 = CARTESIAN_POINT ( 'NONE',  ( 3.752267015613588906E-15, 29.16250000000000142, 4.381197846482986158 ) ) ;
#13900 = CARTESIAN_POINT ( 'NONE',  ( -3.756430356249997438, 25.51562499938548356, 11.16877607737301048 ) ) ;
#13901 = ADVANCED_FACE ( 'NONE', ( #16605 ), #12810, .F. ) ;
#13902 = CARTESIAN_POINT ( 'NONE',  ( 4.000000000000001776, 25.00000000000000000, 8.999999999999992895 ) ) ;
#13903 = CYLINDRICAL_SURFACE ( 'NONE', #12927, 6.000000000000000888 ) ;
#13904 = CARTESIAN_POINT ( 'NONE',  ( 23.35011927068743276, 18.03772451476861605, 11.16877607737301226 ) ) ;
#13905 = DIRECTION ( 'NONE',  ( 0.000000000000000000, 0.000000000000000000, 1.000000000000000000 ) ) ;
#13906 = AXIS2_PLACEMENT_3D ( 'NONE', #2989, #1279, #11340 ) ;
#13907 = DIRECTION ( 'NONE',  ( 1.000000000000000000, 0.000000000000000000, 0.000000000000000000 ) ) ;
#13908 = APPLICATION_PROTOCOL_DEFINITION ( 'draft international standard', 'automotive_design', 1998, #16627 ) ;
#13909 = CARTESIAN_POINT ( 'NONE',  ( -3.999999999999996447, 29.27500000000000213, 8.999999999999992895 ) ) ;
#13910 = CARTESIAN_POINT ( 'NONE',  ( 3.756430356250003211, -6.831223922626973533, 0.2906249993854817526 ) ) ;
#13911 = VECTOR ( 'NONE', #7317, 1000.000000000000000 ) ;
#13912 = CARTESIAN_POINT ( 'NONE',  ( 20.64088888413907696, 20.64088888413900236, 13.33755215474603162 ) ) ;
#13913 = DIRECTION ( 'NONE',  ( 0.000000000000000000, 1.000000000000000000, 0.000000000000000000 ) ) ;
#13914 = ORIENTED_EDGE ( 'NONE', *, *, #25003, .F. ) ;
#13915 = VERTEX_POINT ( 'NONE', #11097 ) ;
#13916 = CARTESIAN_POINT ( 'NONE',  ( 1.999999999999998224, 29.36874999877097636, 12.46410161513774817 ) ) ;
#13917 = ORIENTED_EDGE ( 'NONE', *, *, #2012, .T. ) ;
#13918 = LINE ( 'NONE', #3701, #21900 ) ;
#13919 = VECTOR ( 'NONE', #11241, 1000.000000000000000 ) ;
#13920 = CARTESIAN_POINT ( 'NONE',  ( 3.735045420075836212E-15, 26.71562499938548640, 4.662447845253954171 ) ) ;
#13921 = CARTESIAN_POINT ( 'NONE',  ( -3.469446951953614189E-15, -30.00000000000000355, 4.999999999999992006 ) ) ;
#13922 = DIRECTION ( 'NONE',  ( 0.000000000000000000, 0.000000000000000000, 1.000000000000000000 ) ) ;
#13923 = ORIENTED_EDGE ( 'NONE', *, *, #20430, .F. ) ;
#13924 = EDGE_LOOP ( 'NONE', ( #20697, #5484, #24440, #3045 ) ) ;
#13925 = AXIS2_PLACEMENT_3D ( 'NONE', #4235, #12214, #20183 ) ;
#13926 = ADVANCED_FACE ( 'NONE', ( #18688 ), #3002, .F. ) ;
#13927 = CARTESIAN_POINT ( 'NONE',  ( -1.999999999999996669, 26.14374999877097494, 12.46410161513774639 ) ) ;
#13928 = ORIENTED_EDGE ( 'NONE', *, *, #20315, .F. ) ;
#13929 = CARTESIAN_POINT ( 'NONE',  ( 0.4995657836784084815, 38.49999999999999289, 14.97916666666666075 ) ) ;
#13930 = CARTESIAN_POINT ( 'NONE',  ( -3.756430356249997882, 27.65312499938548640, 11.16877607737301226 ) ) ;
#13931 = CARTESIAN_POINT ( 'NONE',  ( -3.756430356249997882, 28.51562499938548711, 8.999999999999992895 ) ) ;
#13932 = EDGE_CURVE ( 'NONE', #15879, #25564, #2740, .T. ) ;
#13933 = DIRECTION ( 'NONE',  ( 0.5877852522924730261, -0.8090169943749474513, 0.000000000000000000 ) ) ;
#13934 = FACE_OUTER_BOUND ( 'NONE', #21659, .T. ) ;
#13935 = CARTESIAN_POINT ( 'NONE',  ( 4.000000000000003553, 28.15000000000000924, 8.999999999999992895 ) ) ;
#13936 =( GEOMETRIC_REPRESENTATION_CONTEXT ( 3 ) GLOBAL_UNCERTAINTY_ASSIGNED_CONTEXT ( ( #22754 ) ) GLOBAL_UNIT_ASSIGNED_CONTEXT ( ( #14774, #18950, #8888 ) ) REPRESENTATION_CONTEXT ( 'NONE', 'WORKASPACE' ) );
#13937 = CARTESIAN_POINT ( 'NONE',  ( 3.756430356250003655, 26.49062499938548498, 8.999999999999992895 ) ) ;
#13938 = CARTESIAN_POINT ( 'NONE',  ( -24.27856662945480792, 19.43607991389014344, 1.000000000000000000 ) ) ;
#13939 = CIRCLE ( 'NONE', #21873, 0.5000000000000002220 ) ;
#13940 = LINE ( 'NONE', #7782, #13736 ) ;
#13941 = CARTESIAN_POINT ( 'NONE',  ( 21.37230246136343581, 18.54387533661716958, 5.535898384862238508 ) ) ;
#13942 = DIRECTION ( 'NONE',  ( -0.000000000000000000, -1.000000000000000000, -0.000000000000000000 ) ) ;
#13943 = FACE_OUTER_BOUND ( 'NONE', #22039, .T. ) ;
#13944 = CYLINDRICAL_SURFACE ( 'NONE', #11223, 0.5000000000000004441 ) ;
#13945 = CARTESIAN_POINT ( 'NONE',  ( -14.54246377227378062, -27.49048467073843227, 1.000000000000000000 ) ) ;
#13946 = EDGE_LOOP ( 'NONE', ( #6702, #21693, #23466, #7061 ) ) ;
#13947 = CARTESIAN_POINT ( 'NONE',  ( 4.000000000000001776, 26.70624999877097139, 11.30940107675849760 ) ) ;
#13948 = EDGE_CURVE ( 'NONE', #6968, #18161, #1155, .T. ) ;
#13949 = CARTESIAN_POINT ( 'NONE',  ( 3.999999999999996447, -27.47499999999999787, 8.999999999999992895 ) ) ;
#13951 = EDGE_LOOP ( 'NONE', ( #15186, #2688, #18664, #6815 ) ) ;
#13950 = CARTESIAN_POINT ( 'NONE',  ( -1.878215178124999829, 27.80312499938548854, 12.25316411605951927 ) ) ;
#13952 = CARTESIAN_POINT ( 'NONE',  ( 2.672651547586948120E-15, 29.64062499938548356, 13.33755215474603162 ) ) ;
#13953 = CARTESIAN_POINT ( 'NONE',  ( 3.469446951953614189E-15, 31.50000000000000000, 8.999999999999992895 ) ) ;
#13954 = DIRECTION ( 'NONE',  ( 1.000000000000000000, 0.000000000000000000, 0.000000000000000000 ) ) ;
#13955 = FACE_OUTER_BOUND ( 'NONE', #25248, .T. ) ;
#13956 = ORIENTED_EDGE ( 'NONE', *, *, #22471, .F. ) ;
#13957 = ORIENTED_EDGE ( 'NONE', *, *, #23689, .F. ) ;
#13958 = CARTESIAN_POINT ( 'NONE',  ( -1.878215178124994722, 26.64062499938549067, 5.746835883940462963 ) ) ;
#13959 = EDGE_CURVE ( 'NONE', #13534, #24264, #18816, .T. ) ;
#13960 = APPLICATION_CONTEXT ( 'automotive_design' ) ;
#13961 = CARTESIAN_POINT ( 'NONE',  ( 1.878215178125000939, -12.25316411605952283, 4.115624999385482319 ) ) ;
#13962 = EDGE_CURVE ( 'NONE', #17313, #17328, #10702, .T. ) ;
#13963 = CARTESIAN_POINT ( 'NONE',  ( -18.68225429291750928, -24.86329371854754200, -6.500000000000000000 ) ) ;
#13964 = ADVANCED_FACE ( 'NONE', ( #15171 ), #25097, .T. ) ;
#13965 = DIRECTION ( 'NONE',  ( 0.000000000000000000, 0.000000000000000000, 1.000000000000000000 ) ) ;
#13966 =( BOUNDED_CURVE ( )  B_SPLINE_CURVE ( 2, ( #7809, #1932, #4013, #2059, #19832, #2196, #8325 ),
 .UNSPECIFIED., .F., .F. ) 
 B_SPLINE_CURVE_WITH_KNOTS ( ( 3, 2, 2, 3 ),
 ( 0.8499999999999998668, 0.8666666666666664742, 0.8833333333333330817, 0.8999999999999996891 ),
 .UNSPECIFIED. ) 
 CURVE ( )  GEOMETRIC_REPRESENTATION_ITEM ( )  RATIONAL_B_SPLINE_CURVE ( ( 1.000000000000000888, 0.8660254037844378194, 1.000000000000000000, 0.8660254037844387076, 1.000000000000000000, 0.8660254037844413721, 0.9999999999999973355 ) ) 
 REPRESENTATION_ITEM ( '' )  );
#13967 = FACE_OUTER_BOUND ( 'NONE', #23784, .T. ) ;
#13968 = CARTESIAN_POINT ( 'NONE',  ( 3.469446951953614189E-15, 35.50000000000000711, 4.999999999999992006 ) ) ;
#13969 = FACE_OUTER_BOUND ( 'NONE', #9851, .T. ) ;
#13970 = CYLINDRICAL_SURFACE ( 'NONE', #9959, 0.5000000000000004441 ) ;
#13971 = CARTESIAN_POINT ( 'NONE',  ( -9.133673601486680838, -29.72853858738275434, -2.750000000000000000 ) ) ;
#13972 = CARTESIAN_POINT ( 'NONE',  ( 21.42091605170094937, 15.76406180220850040, 8.999999999999992895 ) ) ;
#13973 = ORIENTED_EDGE ( 'NONE', *, *, #21773, .T. ) ;
#13974 = DIRECTION ( 'NONE',  ( 1.000000000000000000, 0.000000000000000000, 0.000000000000000000 ) ) ;
#13975 = CARTESIAN_POINT ( 'NONE',  ( 5.362893858306010841, 38.69544407654356633, 6.779098926265750613 ) ) ;
#13976 = CARTESIAN_POINT ( 'NONE',  ( 2.672651547586948120E-15, 27.39062499938548356, 13.33755215474602984 ) ) ;
#13977 = CARTESIAN_POINT ( 'NONE',  ( -1.289143957944685281, 29.97326948525437729, 12.79562863665509553 ) ) ;
#13978 = CARTESIAN_POINT ( 'NONE',  ( -1.071796769724485454, 26.61115380933863150, 12.99999999999999467 ) ) ;
#13979 = DIRECTION ( 'NONE',  ( -0.7071067811865487940, -0.7071067811865463515, 0.000000000000000000 ) ) ;
#13980 = ORIENTED_EDGE ( 'NONE', *, *, #14998, .T. ) ;
#13981 = DIRECTION ( 'NONE',  ( -0.000000000000000000, -0.000000000000000000, 1.000000000000000000 ) ) ;
#13982 = PLANE ( 'NONE',  #21518 ) ;
#13983 = CARTESIAN_POINT ( 'NONE',  ( -1.626862140677534194E-14, -27.98124999877096997, 12.99999999999999289 ) ) ;
#13985 = EDGE_LOOP ( 'NONE', ( #16685, #15105, #14016, #20542 ) ) ;
#13984 = CARTESIAN_POINT ( 'NONE',  ( 2.000000000000005329, 28.61874999877097281, 5.535898384862238508 ) ) ;
#13986 = ORIENTED_EDGE ( 'NONE', *, *, #4067, .F. ) ;
#13987 = ORIENTED_EDGE ( 'NONE', *, *, #17014, .F. ) ;
#13988 = VERTEX_POINT ( 'NONE', #22756 ) ;
#13989 = CYLINDRICAL_SURFACE ( 'NONE', #13067, 31.10000000000000142 ) ;
#13990 = CARTESIAN_POINT ( 'NONE',  ( -3.034740478393307406, 38.86679461760645182, 13.74602361519018068 ) ) ;
#13991 = SURFACE_STYLE_USAGE ( .BOTH. , #23789 ) ;
#13992 = CARTESIAN_POINT ( 'NONE',  ( 3.756430356250003211, 27.39062499938548711, 8.999999999999992895 ) ) ;
#13993 = CARTESIAN_POINT ( 'NONE',  ( 3.735045420075836212E-15, -4.662447845253954171, 3.403124999385483296 ) ) ;
#13994 = CARTESIAN_POINT ( 'NONE',  ( 3.752267015613588906E-15, -4.381197846482986158, 3.656249998770967569 ) ) ;
#13995 = SHAPE_REPRESENTATION_RELATIONSHIP ( 'NONE' , 'NONE' ,  #20528, #22510 ) ;
#13996 = EDGE_CURVE ( 'NONE', #9053, #12491, #10024, .T. ) ;
#13997 = CARTESIAN_POINT ( 'NONE',  ( 3.735045420075836212E-15, 28.06562499938548427, 4.662447845253954171 ) ) ;
#13998 = EDGE_CURVE ( 'NONE', #20149, #8491, #3262, .T. ) ;
#13999 = CARTESIAN_POINT ( 'NONE',  ( 3.469446951953614189E-15, 35.50000000000000711, 4.999999999999992006 ) ) ;
#14000 = CARTESIAN_POINT ( 'NONE',  ( 8.831537335106614961E-15, 26.63124999877096855, 12.99999999999999112 ) ) ;
#14001 = CARTESIAN_POINT ( 'NONE',  ( -1.878215178124995832, 27.09062499938548640, 5.746835883940462963 ) ) ;
#14002 = FACE_OUTER_BOUND ( 'NONE', #4331, .T. ) ;
#14003 = DIRECTION ( 'NONE',  ( 1.000000000000000000, 0.000000000000000000, 0.000000000000000000 ) ) ;
#14004 = DIRECTION ( 'NONE',  ( -0.000000000000000000, -1.000000000000000000, -0.000000000000000000 ) ) ;
#14005 = CARTESIAN_POINT ( 'NONE',  ( -4.000000000000003553, -29.44374999877096855, 8.999999999999992895 ) ) ;
#14006 = EDGE_CURVE ( 'NONE', #18011, #19944, #6290, .T. ) ;
#14007 = CARTESIAN_POINT ( 'NONE',  ( 3.756430356250002323, 28.36562499938548854, 11.16877607737301226 ) ) ;
#14008 = DIRECTION ( 'NONE',  ( 0.000000000000000000, 0.000000000000000000, 1.000000000000000000 ) ) ;
#14009 = EDGE_CURVE ( 'NONE', #674, #14282, #16314, .T. ) ;
#14010 = MANIFOLD_SOLID_BREP ( 'Cavity1', #23820 ) ;
#14011 = CARTESIAN_POINT ( 'NONE',  ( 4.000000000000003553, -8.999999999999992895, 1.799999999999999600 ) ) ;
#14012 = CARTESIAN_POINT ( 'NONE',  ( 3.469446951953614189E-15, -8.999999999999992895, -10.00000000000000000 ) ) ;
#14013 = ORIENTED_EDGE ( 'NONE', *, *, #8635, .F. ) ;
#14014 = DIRECTION ( 'NONE',  ( 0.000000000000000000, 0.000000000000000000, 1.000000000000000000 ) ) ;
#14016 = ORIENTED_EDGE ( 'NONE', *, *, #22549, .F. ) ;
#14015 = CARTESIAN_POINT ( 'NONE',  ( 4.143002691484658293E-15, 34.00000000000000000, 14.49999999999999289 ) ) ;
#14017 = VERTEX_POINT ( 'NONE', #3512 ) ;
#14018 = CARTESIAN_POINT ( 'NONE',  ( 0.000000000000000000, 0.000000000000000000, 19.59999999999999787 ) ) ;
#14019 = EDGE_CURVE ( 'NONE', #24045, #7204, #14222, .T. ) ;
#14020 = ORIENTED_EDGE ( 'NONE', *, *, #3778, .T. ) ;
#14021 = ORIENTED_EDGE ( 'NONE', *, *, #3069, .F. ) ;
#14022 = EDGE_LOOP ( 'NONE', ( #13024, #7643, #2487, #11236 ) ) ;
#14023 = CARTESIAN_POINT ( 'NONE',  ( 4.000000000000003553, 25.43124999877097281, 6.690598923241489970 ) ) ;
#14024 = ORIENTED_EDGE ( 'NONE', *, *, #3740, .F. ) ;
#14025 = AXIS2_PLACEMENT_3D ( 'NONE', #2152, #10119, #18119 ) ;
#14026 = CARTESIAN_POINT ( 'NONE',  ( 30.12293631110045311, 7.734255490826897450, -6.500000000000000000 ) ) ;
#14027 = CARTESIAN_POINT ( 'NONE',  ( -3.756430356249996994, 25.47812499938548569, 8.999999999999992895 ) ) ;
#14028 = DIRECTION ( 'NONE',  ( 1.000000000000000000, 0.000000000000000000, 0.000000000000000000 ) ) ;
#14029 = CARTESIAN_POINT ( 'NONE',  ( 4.000000000000002665, 25.86250000000000071, 11.30940107675849760 ) ) ;
#14030 = AXIS2_PLACEMENT_3D ( 'NONE', #680, #24864, #2760 ) ;
#14031 = CARTESIAN_POINT ( 'NONE',  ( 17.29753586877772520, 19.95373324673703408, 12.25316411605951927 ) ) ;
#14032 = PLANE ( 'NONE',  #10459 ) ;
#14033 = EDGE_CURVE ( 'NONE', #14041, #23505, #9624, .T. ) ;
#14034 = CARTESIAN_POINT ( 'NONE',  ( -3.999999999999996447, 27.92500000000000071, 8.999999999999992895 ) ) ;
#14035 = CARTESIAN_POINT ( 'NONE',  ( 3.756430356250003655, 28.74062499938548498, 8.999999999999992895 ) ) ;
#14036 = DIRECTION ( 'NONE',  ( 0.000000000000000000, 1.000000000000000000, 0.000000000000000000 ) ) ;
#14037 = CARTESIAN_POINT ( 'NONE',  ( 20.79998790990604718, 20.79998790990596902, 4.662447845253954171 ) ) ;
#14038 = DIRECTION ( 'NONE',  ( -0.000000000000000000, 0.000000000000000000, 1.000000000000000000 ) ) ;
#14039 = VECTOR ( 'NONE', #8110, 1000.000000000000000 ) ;
#14040 = ORIENTED_EDGE ( 'NONE', *, *, #17162, .F. ) ;
#14041 = VERTEX_POINT ( 'NONE', #11602 ) ;
#14042 = CARTESIAN_POINT ( 'NONE',  ( -2.003086131649545506E-15, 26.49062499938548143, 13.33755215474602984 ) ) ;
#14043 = EDGE_CURVE ( 'NONE', #12524, #16720, #12976, .T. ) ;
#14044 = EDGE_LOOP ( 'NONE', ( #2397, #20537, #5282, #20793 ) ) ;
#14045 = DIRECTION ( 'NONE',  ( 0.000000000000000000, 0.000000000000000000, 1.000000000000000000 ) ) ;
#14046 = CARTESIAN_POINT ( 'NONE',  ( 2.672651547586948120E-15, 25.59062499938548640, 13.33755215474602984 ) ) ;
#14047 = CARTESIAN_POINT ( 'NONE',  ( 18.51293941407127974, 18.51293941407120869, 12.99999999999999112 ) ) ;
#14048 = CARTESIAN_POINT ( 'NONE',  ( 0.000000000000000000, 0.000000000000000000, -6.500000000000000000 ) ) ;
#14049 = ORIENTED_EDGE ( 'NONE', *, *, #19996, .T. ) ;
#14050 = DIRECTION ( 'NONE',  ( 0.000000000000000000, 0.000000000000000000, -1.000000000000000000 ) ) ;
#14051 = ORIENTED_EDGE ( 'NONE', *, *, #18537, .T. ) ;
#14052 = CARTESIAN_POINT ( 'NONE',  ( 0.000000000000000000, 0.000000000000000000, -6.500000000000000000 ) ) ;
#14053 = CARTESIAN_POINT ( 'NONE',  ( 3.756430356250002323, 27.80312499938548143, 11.16877607737301226 ) ) ;
#14054 = CARTESIAN_POINT ( 'NONE',  ( 0.000000000000000000, 0.000000000000000000, -6.500000000000000000 ) ) ;
#14055 = CARTESIAN_POINT ( 'NONE',  ( 0.07783014623661463349, 38.99999999999949551, 3.499999999999539479 ) ) ;
#14056 = DIRECTION ( 'NONE',  ( -0.000000000000000000, -0.000000000000000000, -1.000000000000000000 ) ) ;
#14057 = CARTESIAN_POINT ( 'NONE',  ( 4.000000000000001776, 29.50000000000000711, 8.999999999999992895 ) ) ;
#14058 = CARTESIAN_POINT ( 'NONE',  ( 5.532151103383247559, 34.50000000000000000, 11.32277940608563149 ) ) ;
#14059 = CARTESIAN_POINT ( 'NONE',  ( -3.999999999999982681, -6.690598923241479312, 0.1875000000000006384 ) ) ;
#14060 = CARTESIAN_POINT ( 'NONE',  ( -3.834746474454188013E-15, -28.65624999877096712, 4.999999999999992006 ) ) ;
#14061 = ADVANCED_FACE ( 'NONE', ( #17638 ), #1679, .T. ) ;
#14062 = CARTESIAN_POINT ( 'NONE',  ( -22.67092431280609688, -21.28941499438201745, 1.000000000000000000 ) ) ;
#14063 = CARTESIAN_POINT ( 'NONE',  ( 21.80540536484019043, 16.14855111534773968, 6.690598923241489970 ) ) ;
#14064 = LINE ( 'NONE', #6836, #20571 ) ;
#14065 = DIRECTION ( 'NONE',  ( -0.000000000000000000, -1.000000000000000000, -0.000000000000000000 ) ) ;
#14066 = CARTESIAN_POINT ( 'NONE',  ( 23.01190630937068349, 17.35505205987822919, 8.999999999999992895 ) ) ;
#14067 = DIRECTION ( 'NONE',  ( -0.000000000000000000, -0.000000000000000000, 1.000000000000000000 ) ) ;
#14068 = CARTESIAN_POINT ( 'NONE',  ( 18.11727402765218287, 23.42966878357085037, 6.831223922626973533 ) ) ;
#14069 = ORIENTED_EDGE ( 'NONE', *, *, #10153, .T. ) ;
#14070 = CARTESIAN_POINT ( 'NONE',  ( -3.999999999999997335, 27.00624999877096499, 11.30940107675849404 ) ) ;
#14071 = DIRECTION ( 'NONE',  ( -0.000000000000000000, -0.000000000000000000, -1.000000000000000000 ) ) ;
#14073 = ORIENTED_EDGE ( 'NONE', *, *, #4824, .F. ) ;
#14072 = CARTESIAN_POINT ( 'NONE',  ( 0.000000000000000000, 27.84062499938549351, 13.33755215474603162 ) ) ;
#14074 = EDGE_CURVE ( 'NONE', #20492, #3679, #3785, .T. ) ;
#14075 = CARTESIAN_POINT ( 'NONE',  ( 1.878215178125000939, 28.77812499938548640, 12.25316411605952283 ) ) ;
#14076 = CARTESIAN_POINT ( 'NONE',  ( -3.469446951953614189E-15, -30.00000000000000355, 8.999999999999992895 ) ) ;
#14077 = DIRECTION ( 'NONE',  ( 0.000000000000000000, 0.000000000000000000, -1.000000000000000000 ) ) ;
#14078 = ORIENTED_EDGE ( 'NONE', *, *, #10670, .F. ) ;
#14079 = ORIENTED_EDGE ( 'NONE', *, *, #19516, .F. ) ;
#14080 = CARTESIAN_POINT ( 'NONE',  ( 3.756430356249996994, -25.47812499938548569, 8.999999999999992895 ) ) ;
#14081 = CARTESIAN_POINT ( 'NONE',  ( 3.756430356250004543, 27.87812499938548783, 6.831223922626973533 ) ) ;
#14082 = DIRECTION ( 'NONE',  ( 0.000000000000000000, 0.000000000000000000, 1.000000000000000000 ) ) ;
#14083 = CARTESIAN_POINT ( 'NONE',  ( -3.756430356249996994, -8.999999999999992895, 3.065624999385483385 ) ) ;
#14084 = FACE_OUTER_BOUND ( 'NONE', #24830, .T. ) ;
#14085 = SURFACE_STYLE_USAGE ( .BOTH. , #6229 ) ;
#14086 = EDGE_CURVE ( 'NONE', #23081, #14590, #23971, .T. ) ;
#14087 = DIRECTION ( 'NONE',  ( -1.000000000000000000, 0.000000000000000000, 0.000000000000000000 ) ) ;
#14088 = DIRECTION ( 'NONE',  ( -0.000000000000000000, 0.000000000000000000, -1.000000000000000000 ) ) ;
#14089 = EDGE_CURVE ( 'NONE', #408, #11825, #17633, .T. ) ;
#14090 = CARTESIAN_POINT ( 'NONE',  ( 19.18911027444997686, 19.18911027444989870, 12.99999999999999112 ) ) ;
#14091 = DIRECTION ( 'NONE',  ( -0.000000000000000000, -0.000000000000000000, 1.000000000000000000 ) ) ;
#14092 = CARTESIAN_POINT ( 'NONE',  ( 7.437084071668728555E-15, 26.63124999877097565, 12.99999999999999112 ) ) ;
#14093 = DIRECTION ( 'NONE',  ( 0.000000000000000000, 0.000000000000000000, 1.000000000000000000 ) ) ;
#14094 = CARTESIAN_POINT ( 'NONE',  ( 16.90427148687188819, 22.56112573636419683, 11.30940107675849404 ) ) ;
#14095 = ORIENTED_EDGE ( 'NONE', *, *, #14893, .F. ) ;
#14096 = CARTESIAN_POINT ( 'NONE',  ( 3.999999999999997335, -27.06250000000000000, 11.30940107675849404 ) ) ;
#14097 = FACE_OUTER_BOUND ( 'NONE', #19474, .T. ) ;
#14098 = CARTESIAN_POINT ( 'NONE',  ( -1.878215178124998497, 25.44062499938548427, 12.25316411605951927 ) ) ;
#14100 = EDGE_CURVE ( 'NONE', #10597, #9053, #23642, .T. ) ;
#14099 = DIRECTION ( 'NONE',  ( 1.000000000000000000, 0.000000000000000000, 0.000000000000000000 ) ) ;
#14101 = CARTESIAN_POINT ( 'NONE',  ( 11.44867358849351113, 28.91604871112461339, 1.000000000000000000 ) ) ;
#14102 = CARTESIAN_POINT ( 'NONE',  ( -3.999999999999966249, -11.30940107675851181, 2.962499999999997691 ) ) ;
#14103 = ORIENTED_EDGE ( 'NONE', *, *, #4123, .T. ) ;
#14104 = CARTESIAN_POINT ( 'NONE',  ( 1.071796769724494114, 26.83615380933863648, 4.999999999999989342 ) ) ;
#14105 = CARTESIAN_POINT ( 'NONE',  ( 2.620986760973688460E-15, 26.18124999877096926, 13.61880215351699874 ) ) ;
#14106 = DIRECTION ( 'NONE',  ( -0.06279051952931542779, -0.9980267284282714479, 0.000000000000000000 ) ) ;
#14108 = ORIENTED_EDGE ( 'NONE', *, *, #11237, .T. ) ;
#14107 = CARTESIAN_POINT ( 'NONE',  ( 3.756430356250003655, 29.64062499938548356, 8.999999999999992895 ) ) ;
#14109 = ADVANCED_FACE ( 'NONE', ( #1294 ), #13464, .F. ) ;
#14110 = ORIENTED_EDGE ( 'NONE', *, *, #25853, .T. ) ;
#14111 = ORIENTED_EDGE ( 'NONE', *, *, #22417, .T. ) ;
#14112 = ADVANCED_FACE ( 'NONE', ( #11355 ), #1548, .T. ) ;
#14113 = ORIENTED_EDGE ( 'NONE', *, *, #9832, .F. ) ;
#14114 = DIRECTION ( 'NONE',  ( 0.000000000000000000, -0.000000000000000000, -1.000000000000000000 ) ) ;
#14115 =( BOUNDED_CURVE ( )  B_SPLINE_CURVE ( 2, ( #15551, #22058, #15934, #21939, #23765, #17639, #5720 ),
 .UNSPECIFIED., .F., .F. ) 
 B_SPLINE_CURVE_WITH_KNOTS ( ( 3, 2, 2, 3 ),
 ( 0.3500000000000000888, 0.3666666666666666963, 0.3833333333333333592, 0.3999999999999999667 ),
 .UNSPECIFIED. ) 
 CURVE ( )  GEOMETRIC_REPRESENTATION_ITEM ( )  RATIONAL_B_SPLINE_CURVE ( ( 0.9999999999999991118, 0.8660254037844395958, 1.000000000000000000, 0.8660254037844387076, 1.000000000000000000, 0.8660254037844391517, 0.9999999999999995559 ) ) 
 REPRESENTATION_ITEM ( '' )  );
#14116 = CARTESIAN_POINT ( 'NONE',  ( 6.009258394948636914E-15, 26.26562499938548356, 4.662447845253954171 ) ) ;
#14117 = AXIS2_PLACEMENT_3D ( 'NONE', #8022, #16008, #23974 ) ;
#14118 = CARTESIAN_POINT ( 'NONE',  ( 1.878215178125006934, 27.91562499938549280, 5.746835883940462963 ) ) ;
#14119 =( BOUNDED_CURVE ( )  B_SPLINE_CURVE ( 2, ( #4839, #11103, #17132, #25103, #20664, #1161, #1300, #13082, #1048 ),
 .UNSPECIFIED., .F., .F. ) 
 B_SPLINE_CURVE_WITH_KNOTS ( ( 3, 2, 2, 2, 3 ),
 ( 0.4750000000000000333, 0.4833333333333333370, 0.5000000000000000000, 0.5166666666666667185, 0.5250000000000000222 ),
 .UNSPECIFIED. ) 
 CURVE ( )  GEOMETRIC_REPRESENTATION_ITEM ( )  RATIONAL_B_SPLINE_CURVE ( ( 0.9330127018922194093, 0.9330127018922196314, 1.000000000000000000, 0.8660254037844387076, 1.000000000000000000, 0.8660254037844387076, 1.000000000000000000, 0.9330127018922194093, 0.9330127018922194093 ) ) 
 REPRESENTATION_ITEM ( '' )  );
#14120 = CARTESIAN_POINT ( 'NONE',  ( 3.756430356250002323, -11.16877607737301226, 4.603124999385482141 ) ) ;
#14121 = CARTESIAN_POINT ( 'NONE',  ( -1.878215178124995832, -5.746835883940462963, 0.4031249993854852942 ) ) ;
#14122 = CARTESIAN_POINT ( 'NONE',  ( 1.878215178125000939, 26.41562499938548214, 12.25316411605952283 ) ) ;
#14123 = LINE ( 'NONE', #4435, #2541 ) ;
#14124 = LINE ( 'NONE', #22089, #8848 ) ;
#14125 = CARTESIAN_POINT ( 'NONE',  ( 3.756430356250003655, 26.94062499938548427, 8.999999999999992895 ) ) ;
#14126 = CYLINDRICAL_SURFACE ( 'NONE', #6712, 31.10000000000000142 ) ;
#14127 = CARTESIAN_POINT ( 'NONE',  ( -4.000000000000003553, -29.89374999877096784, 8.999999999999992895 ) ) ;
#14128 = DIRECTION ( 'NONE',  ( -0.6845471059286901694, -0.7289686274214101092, 0.000000000000000000 ) ) ;
#14129 = CARTESIAN_POINT ( 'NONE',  ( -3.735045420075836212E-15, -25.36562499938548498, 4.662447845253954171 ) ) ;
#14130 = CARTESIAN_POINT ( 'NONE',  ( 3.756430356250003655, 27.95312499938548711, 8.999999999999992895 ) ) ;
#14131 = DIRECTION ( 'NONE',  ( 0.000000000000000000, 0.000000000000000000, 1.000000000000000000 ) ) ;
#14132 = AXIS2_PLACEMENT_3D ( 'NONE', #14688, #2518, #10225 ) ;
#14133 = CARTESIAN_POINT ( 'NONE',  ( 1.071796769724496334, 28.18615380933863435, 4.999999999999992895 ) ) ;
#14134 = ADVANCED_BREP_SHAPE_REPRESENTATION ( '', ( #4848, #21036 ), #8093 ) ;
#14135 = DIRECTION ( 'NONE',  ( -0.000000000000000000, -0.000000000000000000, 1.000000000000000000 ) ) ;
#14137 = EDGE_LOOP ( 'NONE', ( #25655, #16723, #24068, #673 ) ) ;
#14136 = PRODUCT_RELATED_PRODUCT_CATEGORY ( 'part', '', ( #2546 ) ) ;
#14138 = CARTESIAN_POINT ( 'NONE',  ( -3.756430356250003655, -29.75312499938548783, 8.999999999999992895 ) ) ;
#14139 = ORIENTED_EDGE ( 'NONE', *, *, #13314, .T. ) ;
#14140 = ORIENTED_EDGE ( 'NONE', *, *, #15011, .T. ) ;
#14142 = ORIENTED_EDGE ( 'NONE', *, *, #16568, .F. ) ;
#14141 = AXIS2_PLACEMENT_3D ( 'NONE', #12972, #1072, #5372 ) ;
#14143 = EDGE_CURVE ( 'NONE', #3077, #15156, #19197, .T. ) ;
#14144 = VERTEX_POINT ( 'NONE', #17761 ) ;
#14145 = ORIENTED_EDGE ( 'NONE', *, *, #24655, .F. ) ;
#14146 = CARTESIAN_POINT ( 'NONE',  ( 26.49999999999999645, -0.5000000000000000000, 19.00000000000000000 ) ) ;
#14147 = ADVANCED_FACE ( 'NONE', ( #21298 ), #7813, .F. ) ;
#14148 = ORIENTED_EDGE ( 'NONE', *, *, #11274, .T. ) ;
#14149 = CARTESIAN_POINT ( 'NONE',  ( 4.000000000000001776, 29.01249999999999929, 11.30940107675849760 ) ) ;
#14150 = CARTESIAN_POINT ( 'NONE',  ( -1.878215178124998497, 27.35312499938548569, 12.25316411605951927 ) ) ;
#14151 = CIRCLE ( 'NONE', #22925, 4.000000000000000000 ) ;
#14152 = CARTESIAN_POINT ( 'NONE',  ( -3.756430356249995661, -6.831223922626973533, 3.590624999385483740 ) ) ;
#14153 = CARTESIAN_POINT ( 'NONE',  ( 3.834746474454188013E-15, 27.75624999877096855, 4.999999999999992006 ) ) ;
#14154 = CARTESIAN_POINT ( 'NONE',  ( 15.91640417120904871, 21.22879892712773042, 8.999999999999992895 ) ) ;
#14155 = CYLINDRICAL_SURFACE ( 'NONE', #12559, 31.10000000000000142 ) ;
#14156 = CIRCLE ( 'NONE', #2877, 31.10000000000000142 ) ;
#14157 = PRESENTATION_STYLE_ASSIGNMENT (( #6437 ) ) ;
#14158 = AXIS2_PLACEMENT_3D ( 'NONE', #23013, #14093, #20099 ) ;
#14159 = CARTESIAN_POINT ( 'NONE',  ( 3.756430356250003655, -8.999999999999992895, 1.490624999385483429 ) ) ;
#14160 = CARTESIAN_POINT ( 'NONE',  ( -3.999999999999997335, 27.51250000000000284, 11.30940107675849404 ) ) ;
#14161 = CARTESIAN_POINT ( 'NONE',  ( 1.878215178125000939, 28.21562499938548640, 12.25316411605952283 ) ) ;
#14162 = CARTESIAN_POINT ( 'NONE',  ( 3.735045420075836212E-15, -4.662447845253954171, 0.3656249993854837621 ) ) ;
#14163 = FACE_OUTER_BOUND ( 'NONE', #23960, .T. ) ;
#14164 = ORIENTED_EDGE ( 'NONE', *, *, #9183, .T. ) ;
#14165 = EDGE_LOOP ( 'NONE', ( #4760, #20, #13601, #8824 ) ) ;
#14166 = CARTESIAN_POINT ( 'NONE',  ( 2.003086131649545506E-15, 25.59062499938548996, 13.33755215474602984 ) ) ;
#14168 = ORIENTED_EDGE ( 'NONE', *, *, #10025, .T. ) ;
#14167 = VECTOR ( 'NONE', #25207, 1000.000000000000000 ) ;
#14169 = DIRECTION ( 'NONE',  ( 0.000000000000000000, 0.000000000000000000, -1.000000000000000000 ) ) ;
#14170 = EDGE_CURVE ( 'NONE', #18087, #3297, #21169, .T. ) ;
#14171 = CARTESIAN_POINT ( 'NONE',  ( -1.999999999999998224, 29.74374999877096926, 12.46410161513774639 ) ) ;
#14172 = CARTESIAN_POINT ( 'NONE',  ( -3.756430356249996994, 29.52812499938548640, 8.999999999999992895 ) ) ;
#14173 = CARTESIAN_POINT ( 'NONE',  ( -1.999999999999998224, 26.20000000000000284, 12.46410161513774639 ) ) ;
#14174 = ORIENTED_EDGE ( 'NONE', *, *, #12318, .T. ) ;
#14176 = ADVANCED_FACE ( 'NONE', ( #11869 ), #13970, .F. ) ;
#14175 = VECTOR ( 'NONE', #2674, 1000.000000000000000 ) ;
#14177 = FACE_OUTER_BOUND ( 'NONE', #4481, .T. ) ;
#14178 = CIRCLE ( 'NONE', #24602, 0.4999999999999983902 ) ;
#14179 = ORIENTED_EDGE ( 'NONE', *, *, #15758, .F. ) ;
#14180 = CARTESIAN_POINT ( 'NONE',  ( -0.4949451094549311425, 38.61079987549954495, 14.86836679116710691 ) ) ;
#14181 = CARTESIAN_POINT ( 'NONE',  ( 3.735045420075836212E-15, 26.15312499938548285, 4.662447845253954171 ) ) ;
#14182 = CARTESIAN_POINT ( 'NONE',  ( 2.000000000000003997, 29.12500000000000000, 5.535898384862238508 ) ) ;
#14183 = AXIS2_PLACEMENT_3D ( 'NONE', #13238, #11525, #17422 ) ;
#14184 = DIRECTION ( 'NONE',  ( -0.9980267284282718920, -0.06279051952930848890, 0.000000000000000000 ) ) ;
#14185 = CARTESIAN_POINT ( 'NONE',  ( -1.057460391440397258E-14, 29.55624999877096926, 4.999999999999992006 ) ) ;
#14186 = CARTESIAN_POINT ( 'NONE',  ( 2.000000000000000000, 29.42500000000000426, 12.46410161513774817 ) ) ;
#14187 = EDGE_CURVE ( 'NONE', #6036, #11726, #23814, .T. ) ;
#14188 = CIRCLE ( 'NONE', #4151, 0.4999999999999999445 ) ;
#14189 = CIRCLE ( 'NONE', #5811, 31.10000000000000142 ) ;
#14190 = AXIS2_PLACEMENT_3D ( 'NONE', #7807, #15927, #24022 ) ;
#14191 = CARTESIAN_POINT ( 'NONE',  ( 1.071796769724488563, -28.86115380933863506, 12.99999999999999289 ) ) ;
#14192 = AXIS2_PLACEMENT_3D ( 'NONE', #16648, #24099, #8281 ) ;
#14193 = DIRECTION ( 'NONE',  ( 0.000000000000000000, 0.000000000000000000, 1.000000000000000000 ) ) ;
#14194 = CARTESIAN_POINT ( 'NONE',  ( -11.44867358849309547, 28.91604871112477326, -6.500000000000000000 ) ) ;
#14195 = CARTESIAN_POINT ( 'NONE',  ( -4.000000000000003553, -28.54374999877096997, 8.999999999999992895 ) ) ;
#14196 = DIRECTION ( 'NONE',  ( 0.000000000000000000, 0.000000000000000000, -1.000000000000000000 ) ) ;
#14197 = CARTESIAN_POINT ( 'NONE',  ( -1.999999999999995781, 25.15000000000000213, 5.535898384862237620 ) ) ;
#14198 = DIRECTION ( 'NONE',  ( 0.000000000000000000, 1.000000000000000000, 0.000000000000000000 ) ) ;
#14199 = AXIS2_PLACEMENT_3D ( 'NONE', #11496, #17277, #25242 ) ;
#14200 = ORIENTED_EDGE ( 'NONE', *, *, #24748, .T. ) ;
#14201 = CARTESIAN_POINT ( 'NONE',  ( 2.620986760973688460E-15, 28.88124999877096855, 13.61880215351699874 ) ) ;
#14202 = CARTESIAN_POINT ( 'NONE',  ( -2.000000000000003997, -28.22500000000000142, 5.535898384862238508 ) ) ;
#14204 = ORIENTED_EDGE ( 'NONE', *, *, #19020, .T. ) ;
#14203 = CARTESIAN_POINT ( 'NONE',  ( -1.878215178124994722, 26.75312499938549138, 5.746835883940462963 ) ) ;
#14205 = EDGE_CURVE ( 'NONE', #18284, #22563, #6091, .T. ) ;
#14206 = CARTESIAN_POINT ( 'NONE',  ( 1.878215178125004048, 28.92812499938548854, 5.746835883940462963 ) ) ;
#14207 = AXIS2_PLACEMENT_3D ( 'NONE', #23673, #5507, #25512 ) ;
#14208 = CARTESIAN_POINT ( 'NONE',  ( 4.000000000000002665, 27.21250000000000568, 11.30940107675849760 ) ) ;
#14209 = CARTESIAN_POINT ( 'NONE',  ( -3.999999999999996447, 27.86874999877096570, 8.999999999999992895 ) ) ;
#14210 = ORIENTED_EDGE ( 'NONE', *, *, #13772, .F. ) ;
#14211 = ORIENTED_EDGE ( 'NONE', *, *, #20030, .F. ) ;
#14212 = CARTESIAN_POINT ( 'NONE',  ( 3.756430356249996994, -27.72812499938548569, 8.999999999999992895 ) ) ;
#14213 = CARTESIAN_POINT ( 'NONE',  ( 3.756430356250004543, 28.70312499938549067, 11.16877607737301226 ) ) ;
#14214 = FACE_OUTER_BOUND ( 'NONE', #2798, .T. ) ;
#14215 = VECTOR ( 'NONE', #22383, 1000.000000000000000 ) ;
#14216 = ADVANCED_FACE ( 'NONE', ( #12380 ), #14227, .F. ) ;
#14217 = CARTESIAN_POINT ( 'NONE',  ( -3.756430356249997438, -11.16877607737301048, 2.653124999385483296 ) ) ;
#14218 = ADVANCED_FACE ( 'NONE', ( #20345 ), #12123, .T. ) ;
#14219 = AXIS2_PLACEMENT_3D ( 'NONE', #9794, #19971, #15563 ) ;
#14220 = CARTESIAN_POINT ( 'NONE',  ( 8.831537335106614961E-15, 27.53124999877097068, 12.99999999999999112 ) ) ;
#14221 = LINE ( 'NONE', #20342, #15438 ) ;
#14222 = CIRCLE ( 'NONE', #19644, 0.4999999999999996669 ) ;
#14223 = AXIS2_PLACEMENT_3D ( 'NONE', #3182, #17322, #25285 ) ;
#14224 = CARTESIAN_POINT ( 'NONE',  ( -28.34936733434213707, -12.78762572734027181, -6.500000000000000000 ) ) ;
#14225 = DIRECTION ( 'NONE',  ( 1.000000000000000000, 0.000000000000000000, 0.000000000000000000 ) ) ;
#14226 = DIRECTION ( 'NONE',  ( -0.000000000000000000, -1.000000000000000000, -0.000000000000000000 ) ) ;
#14227 = CYLINDRICAL_SURFACE ( 'NONE', #1620, 4.000000000000000000 ) ;
#14228 = CARTESIAN_POINT ( 'NONE',  ( 18.14606400620158411, 20.80226138416088588, 5.746835883940462963 ) ) ;
#14229 = CARTESIAN_POINT ( 'NONE',  ( 21.54465973840859760, 18.71623261366233848, 12.46410161513774817 ) ) ;
#14230 = CIRCLE ( 'NONE', #2953, 0.5000000000000007772 ) ;
#14231 = ORIENTED_EDGE ( 'NONE', *, *, #1844, .T. ) ;
#14232 = DIRECTION ( 'NONE',  ( 0.000000000000000000, 0.000000000000000000, 1.000000000000000000 ) ) ;
#14233 = CARTESIAN_POINT ( 'NONE',  ( 1.294650675951837693, 29.97301818707614984, 5.206367449752296039 ) ) ;
#14234 = CARTESIAN_POINT ( 'NONE',  ( -1.878215178124998497, 25.89062499938548356, 12.25316411605951927 ) ) ;
#14235 = CIRCLE ( 'NONE', #6297, 6.000000000000000000 ) ;
#14237 = ORIENTED_EDGE ( 'NONE', *, *, #6750, .F. ) ;
#14236 = CARTESIAN_POINT ( 'NONE',  ( -3.595408253811773758, 29.78394301743083261, 10.77252090037689136 ) ) ;
#14238 = CARTESIAN_POINT ( 'NONE',  ( -23.96296185032722548, -19.82388608118403539, 1.000000000000000000 ) ) ;
#14239 = CARTESIAN_POINT ( 'NONE',  ( 30.54913349766223973, 5.827558883615938434, -6.500000000000000000 ) ) ;
#14240 = EDGE_LOOP ( 'NONE', ( #17690, #8445, #17476, #6292 ) ) ;
#14241 = DIRECTION ( 'NONE',  ( 0.000000000000000000, 0.000000000000000000, -1.000000000000000000 ) ) ;
#14242 = CARTESIAN_POINT ( 'NONE',  ( -3.999999999999996447, 26.51874999877097139, 8.999999999999992895 ) ) ;
#14243 = CARTESIAN_POINT ( 'NONE',  ( -2.672651547586948120E-15, -27.27812499938548285, 13.33755215474602984 ) ) ;
#14245 = ORIENTED_EDGE ( 'NONE', *, *, #21962, .F. ) ;
#14244 = CARTESIAN_POINT ( 'NONE',  ( 5.706339097770919189, 29.50000000000000000, 7.145898033750285983 ) ) ;
#14246 = CIRCLE ( 'NONE', #17580, 31.10000000000000142 ) ;
#14247 = EDGE_LOOP ( 'NONE', ( #8106, #24980, #5116, #13186 ) ) ;
#14248 = ORIENTED_EDGE ( 'NONE', *, *, #9037, .T. ) ;
#14249 = ORIENTED_EDGE ( 'NONE', *, *, #25156, .T. ) ;
#14250 = DIRECTION ( 'NONE',  ( -0.9048270524660229075, -0.4257792915650654986, 0.000000000000000000 ) ) ;
#14251 = CIRCLE ( 'NONE', #5462, 31.10000000000000142 ) ;
#14252 = CARTESIAN_POINT ( 'NONE',  ( 3.756430356250003211, 25.70312499938548356, 8.999999999999992895 ) ) ;
#14253 = VECTOR ( 'NONE', #22124, 1000.000000000000000 ) ;
#14254 = EDGE_CURVE ( 'NONE', #5166, #1446, #25414, .T. ) ;
#14255 = CARTESIAN_POINT ( 'NONE',  ( -28.91604871112473418, -11.44867358849319849, -6.500000000000000000 ) ) ;
#14256 = CIRCLE ( 'NONE', #22180, 31.10000000000000142 ) ;
#14257 = EDGE_CURVE ( 'NONE', #14559, #8133, #13276, .T. ) ;
#14258 = DIRECTION ( 'NONE',  ( 1.000000000000000000, 0.000000000000000000, 0.000000000000000000 ) ) ;
#14259 = CARTESIAN_POINT ( 'NONE',  ( 2.620986760973688460E-15, -13.61880215351699874, 4.331249998770966059 ) ) ;
#14260 = SURFACE_SIDE_STYLE ('',( #529 ) ) ;
#14261 = CARTESIAN_POINT ( 'NONE',  ( 1.878215178125000939, 26.86562499938548498, 12.25316411605952283 ) ) ;
#14262 = CARTESIAN_POINT ( 'NONE',  ( 1.500000000000001776, -10.49999999999999289, -6.938893903907228378E-15 ) ) ;
#14263 = AXIS2_PLACEMENT_3D ( 'NONE', #15756, #23720, #19918 ) ;
#14264 = DIRECTION ( 'NONE',  ( -0.000000000000000000, -1.000000000000000000, -0.000000000000000000 ) ) ;
#14265 = CARTESIAN_POINT ( 'NONE',  ( -3.756430356249997438, 25.40312499938548285, 11.16877607737301048 ) ) ;
#14266 = CARTESIAN_POINT ( 'NONE',  ( -31.09598070739550124, 0.4999838450263022760, -2.750000000000000000 ) ) ;
#14268 = EDGE_CURVE ( 'NONE', #3560, #9004, #3276, .T. ) ;
#14267 = CARTESIAN_POINT ( 'NONE',  ( 3.878215178125003604, -8.999999999999992895, 0.07031249969274150358 ) ) ;
#14269 = DIRECTION ( 'NONE',  ( 1.000000000000000000, 0.000000000000000000, 0.000000000000000000 ) ) ;
#14270 = CARTESIAN_POINT ( 'NONE',  ( 1.999999999999998224, -28.39374999877096784, 12.46410161513774639 ) ) ;
#14271 = AXIS2_PLACEMENT_3D ( 'NONE', #17601, #17470, #1647 ) ;
#14272 = CARTESIAN_POINT ( 'NONE',  ( 27.92360179968367362, -13.69242354489163027, -2.750000000000000000 ) ) ;
#14273 = VECTOR ( 'NONE', #24749, 1000.000000000000000 ) ;
#14274 = CARTESIAN_POINT ( 'NONE',  ( 3.469446951953614189E-15, 38.49999999999999289, 8.999999999999992895 ) ) ;
#14275 = DIRECTION ( 'NONE',  ( 0.000000000000000000, 0.000000000000000000, 1.000000000000000000 ) ) ;
#14276 = DIRECTION ( 'NONE',  ( 0.000000000000000000, -0.000000000000000000, 1.000000000000000000 ) ) ;
#14277 = ORIENTED_EDGE ( 'NONE', *, *, #5142, .F. ) ;
#14278 = LINE ( 'NONE', #20389, #5824 ) ;
#14280 = ORIENTED_EDGE ( 'NONE', *, *, #24238, .F. ) ;
#14279 = FACE_OUTER_BOUND ( 'NONE', #6700, .T. ) ;
#14281 =( BOUNDED_CURVE ( )  B_SPLINE_CURVE ( 2, ( #9748, #5688, #21779, #20060, #5815, #24115, #6199 ),
 .UNSPECIFIED., .F., .F. ) 
 B_SPLINE_CURVE_WITH_KNOTS ( ( 3, 2, 2, 3 ),
 ( 0.1499999999999996891, 0.1666666666666665741, 0.1833333333333334592, 0.2000000000000003719 ),
 .UNSPECIFIED. ) 
 CURVE ( )  GEOMETRIC_REPRESENTATION_ITEM ( )  RATIONAL_B_SPLINE_CURVE ( ( 1.000000000000002665, 0.8660254037844363761, 1.000000000000000000, 0.8660254037844387076, 1.000000000000000000, 0.8660254037844358210, 1.000000000000002887 ) ) 
 REPRESENTATION_ITEM ( '' )  );
#14282 = VERTEX_POINT ( 'NONE', #500 ) ;
#14283 = VERTEX_POINT ( 'NONE', #15933 ) ;
#14284 = ADVANCED_FACE ( 'NONE', ( #9899 ), #17885, .T. ) ;
#14285 = EDGE_LOOP ( 'NONE', ( #21888, #1558, #11289, #20820 ) ) ;
#14286 = ORIENTED_EDGE ( 'NONE', *, *, #19626, .T. ) ;
#14287 = CARTESIAN_POINT ( 'NONE',  ( 20.72827001538724900, 19.21252048753512298, 4.999999999999992895 ) ) ;
#14288 =( BOUNDED_CURVE ( )  B_SPLINE_CURVE ( 2, ( #24939, #3107, #12520, #1135, #6897, #8871, #18936, #4540, #9108 ),
 .UNSPECIFIED., .F., .F. ) 
 B_SPLINE_CURVE_WITH_KNOTS ( ( 3, 2, 2, 2, 3 ),
 ( 0.8250000000000000666, 0.8333333333333333703, 0.8499999999999999778, 0.8666666666666666963, 0.8750000000000000000 ),
 .UNSPECIFIED. ) 
 CURVE ( )  GEOMETRIC_REPRESENTATION_ITEM ( )  RATIONAL_B_SPLINE_CURVE ( ( 0.9330127018922194093, 0.9330127018922198534, 1.000000000000000000, 0.8660254037844387076, 1.000000000000000000, 0.8660254037844387076, 1.000000000000000000, 0.9330127018922194093, 0.9330127018922194093 ) ) 
 REPRESENTATION_ITEM ( '' )  );
#14289 = AXIS2_PLACEMENT_3D ( 'NONE', #22717, #12891, #19986 ) ;
#14290 = ORIENTED_EDGE ( 'NONE', *, *, #24055, .F. ) ;
#14291 = CYLINDRICAL_SURFACE ( 'NONE', #8166, 0.5000000000000004441 ) ;
#14292 = CARTESIAN_POINT ( 'NONE',  ( -1.878215178124995832, 26.30312499938548498, 5.746835883940462963 ) ) ;
#14293 = AXIS2_PLACEMENT_3D ( 'NONE', #396, #2232, #6018 ) ;
#14294 = CARTESIAN_POINT ( 'NONE',  ( -3.756430356249997882, -11.16877607737301226, 3.215624999385481964 ) ) ;
#14295 = CARTESIAN_POINT ( 'NONE',  ( -20.20656826142290541, -23.64116323484223869, 1.000000000000000000 ) ) ;
#14296 = CARTESIAN_POINT ( 'NONE',  ( 19.12944813935283150, 19.12944813935275334, 4.662447845253954171 ) ) ;
#14297 = EDGE_CURVE ( 'NONE', #18150, #22371, #21938, .T. ) ;
#14298 = VECTOR ( 'NONE', #8273, 1000.000000000000000 ) ;
#14299 = CARTESIAN_POINT ( 'NONE',  ( 17.52740933866159168, 23.18426358815389676, 6.690598923241487306 ) ) ;
#14300 = DIRECTION ( 'NONE',  ( 1.000000000000000000, 0.000000000000000000, -0.000000000000000000 ) ) ;
#14301 = CARTESIAN_POINT ( 'NONE',  ( -1.878215178124998497, -12.25316411605951927, 2.240624999385484095 ) ) ;
#14302 = ADVANCED_FACE ( 'NONE', ( #19958 ), #14870, .F. ) ;
#14303 = CARTESIAN_POINT ( 'NONE',  ( -29.72853858738291422, -9.133673601486165694, -6.500000000000000000 ) ) ;
#14304 = CARTESIAN_POINT ( 'NONE',  ( 1.878215178125004048, 28.36562499938548143, 5.746835883940462963 ) ) ;
#14305 = EDGE_CURVE ( 'NONE', #1228, #22272, #15789, .T. ) ;
#14306 = CARTESIAN_POINT ( 'NONE',  ( 3.756430356250002323, -11.16877607737301403, 1.115624999385483429 ) ) ;
#14307 = CARTESIAN_POINT ( 'NONE',  ( -3.999999999999995559, 27.43750000000000000, 6.690598923241487306 ) ) ;
#14308 = CARTESIAN_POINT ( 'NONE',  ( 1.859271017917182139E-15, 29.38749999999999929, 12.99999999999999289 ) ) ;
#14309 = CIRCLE ( 'NONE', #17635, 0.5000000000000001110 ) ;
#14310 = ORIENTED_EDGE ( 'NONE', *, *, #9465, .F. ) ;
#14311 = ORIENTED_EDGE ( 'NONE', *, *, #4172, .T. ) ;
#14312 = CARTESIAN_POINT ( 'NONE',  ( 6.009258394948636914E-15, 27.61562499938548854, 4.662447845253954171 ) ) ;
#14313 = CIRCLE ( 'NONE', #1779, 31.10000000000000142 ) ;
#14314 = AXIS2_PLACEMENT_3D ( 'NONE', #10834, #1296, #17265 ) ;
#14315 = VERTEX_POINT ( 'NONE', #14744 ) ;
#14316 = CARTESIAN_POINT ( 'NONE',  ( 17.08421000182766747, 25.98730014090443063, 1.000000000000000000 ) ) ;
#14317 = ORIENTED_EDGE ( 'NONE', *, *, #19887, .T. ) ;
#14318 = LINE ( 'NONE', #2396, #16747 ) ;
#14319 = VERTEX_POINT ( 'NONE', #24418 ) ;
#14320 = DIRECTION ( 'NONE',  ( -1.000000000000000000, 2.891205793294678326E-16, 0.000000000000000000 ) ) ;
#14321 = ORIENTED_EDGE ( 'NONE', *, *, #17409, .T. ) ;
#14322 = CYLINDRICAL_SURFACE ( 'NONE', #137, 1.000000000000000000 ) ;
#14323 = CARTESIAN_POINT ( 'NONE',  ( 3.756430356250002323, 28.25312499938548427, 11.16877607737301226 ) ) ;
#14324 = FACE_OUTER_BOUND ( 'NONE', #13951, .T. ) ;
#14325 = CIRCLE ( 'NONE', #13906, 6.000000000000000000 ) ;
#14326 = CARTESIAN_POINT ( 'NONE',  ( 4.000000000000003553, 26.83749999999999503, 6.690598923241489970 ) ) ;
#14327 = DIRECTION ( 'NONE',  ( 1.000000000000000000, 0.000000000000000000, 0.000000000000000000 ) ) ;
#14328 = CARTESIAN_POINT ( 'NONE',  ( 4.000000000000002665, 29.73213749463701205, 9.470295877454901756 ) ) ;
#14329 = CIRCLE ( 'NONE', #11381, 0.5000000000000004441 ) ;
#14330 = EDGE_CURVE ( 'NONE', #6385, #21955, #13312, .T. ) ;
#14331 = CARTESIAN_POINT ( 'NONE',  ( 3.756430356250004099, 27.42812499938548143, 6.831223922626973533 ) ) ;
#14332 = EDGE_CURVE ( 'NONE', #4508, #2838, #11638, .T. ) ;
#14333 = DIRECTION ( 'NONE',  ( 0.000000000000000000, 1.000000000000000000, 0.000000000000000000 ) ) ;
#14334 = CARTESIAN_POINT ( 'NONE',  ( -0.4860084296119258074, 38.61007524145222192, 3.130138664374117585 ) ) ;
#14335 = CARTESIAN_POINT ( 'NONE',  ( -1.071796769724488563, 29.36740381056767291, 12.99999999999999289 ) ) ;
#14336 = EDGE_CURVE ( 'NONE', #5148, #6810, #14995, .T. ) ;
#14337 = CARTESIAN_POINT ( 'NONE',  ( 1.071796769724487230, -27.77634618820330559, 4.999999999999992006 ) ) ;
#14338 = LINE ( 'NONE', #23877, #6223 ) ;
#14339 = DIRECTION ( 'NONE',  ( 0.000000000000000000, 0.000000000000000000, 1.000000000000000000 ) ) ;
#14340 = ORIENTED_EDGE ( 'NONE', *, *, #22902, .T. ) ;
#14341 = CARTESIAN_POINT ( 'NONE',  ( 2.620986760973688460E-15, 27.98124999877096997, 13.61880215351699874 ) ) ;
#14342 = CARTESIAN_POINT ( 'NONE',  ( 3.999999999999996003, -28.78750000000000142, 6.690598923241487306 ) ) ;
#14344 = ORIENTED_EDGE ( 'NONE', *, *, #20315, .T. ) ;
#14343 = CARTESIAN_POINT ( 'NONE',  ( 1.878215178124999829, 28.32812499938549422, 12.25316411605952283 ) ) ;
#14345 = ORIENTED_EDGE ( 'NONE', *, *, #11954, .F. ) ;
#14346 = CARTESIAN_POINT ( 'NONE',  ( -3.999999999999996447, 28.76874999877096784, 8.999999999999992895 ) ) ;
#14347 = CARTESIAN_POINT ( 'NONE',  ( 0.000000000000000000, 0.000000000000000000, -6.500000000000000000 ) ) ;
#14348 = CARTESIAN_POINT ( 'NONE',  ( 3.959305671612554781E-15, 40.00000000000000000, 12.99999999999999289 ) ) ;
#14349 = VERTEX_POINT ( 'NONE', #12508 ) ;
#14350 = VERTEX_POINT ( 'NONE', #5061 ) ;
#14351 = CARTESIAN_POINT ( 'NONE',  ( -3.756430356250002323, -26.56562499938548783, 11.16877607737301403 ) ) ;
#14352 = CARTESIAN_POINT ( 'NONE',  ( 1.878215178125003382, 27.01562499938548711, 5.746835883940462963 ) ) ;
#14353 = DIRECTION ( 'NONE',  ( -1.000000000000000000, 0.000000000000000000, 0.000000000000000000 ) ) ;
#14354 = MECHANICAL_DESIGN_GEOMETRIC_PRESENTATION_REPRESENTATION (  '', ( #2661 ), #20630 ) ;
#14355 = FACE_OUTER_BOUND ( 'NONE', #12826, .T. ) ;
#14356 = CIRCLE ( 'NONE', #15610, 0.5000000000000019984 ) ;
#14357 = CARTESIAN_POINT ( 'NONE',  ( -1.999999999999995781, -5.535898384862237620, 3.300000000000000711 ) ) ;
#14358 = EDGE_CURVE ( 'NONE', #9527, #14695, #19453, .T. ) ;
#14359 = CARTESIAN_POINT ( 'NONE',  ( 0.000000000000000000, 0.000000000000000000, -6.500000000000000000 ) ) ;
#14360 = EDGE_CURVE ( 'NONE', #17588, #7360, #24533, .T. ) ;
#14361 = DIRECTION ( 'NONE',  ( -0.7071067811865487940, -0.7071067811865463515, 0.000000000000000000 ) ) ;
#14362 = DIRECTION ( 'NONE',  ( -0.000000000000000000, -0.000000000000000000, 1.000000000000000000 ) ) ;
#14363 = CARTESIAN_POINT ( 'NONE',  ( 20.78010053211970032, 20.78010053211962926, 12.99999999999999289 ) ) ;
#14364 = CARTESIAN_POINT ( 'NONE',  ( 19.68856820379214057, 17.03237082583270023, 12.25316411605952283 ) ) ;
#14365 = CARTESIAN_POINT ( 'NONE',  ( 20.10392967174101031, 20.10392967174093926, 13.61880215351699874 ) ) ;
#14366 = ORIENTED_EDGE ( 'NONE', *, *, #1536, .F. ) ;
#14367 = CARTESIAN_POINT ( 'NONE',  ( -19.43607991388963896, 24.27856662945520583, 1.000000000000000000 ) ) ;
#14368 = CARTESIAN_POINT ( 'NONE',  ( 5.218530426542799638, 39.00437929243753388, 7.275652536849361418 ) ) ;
#14369 = CARTESIAN_POINT ( 'NONE',  ( -3.756430356249997882, 26.30312499938548498, 11.16877607737301226 ) ) ;
#14371 = VERTEX_POINT ( 'NONE', #11063 ) ;
#14370 = CARTESIAN_POINT ( 'NONE',  ( 21.21320343559646915, 21.21320343559638744, 4.999999999999992006 ) ) ;
#14372 = COLOUR_RGB ( '',0.8941176470588234615, 0.8941176470588234615, 0.8941176470588234615 ) ;
#14373 = CARTESIAN_POINT ( 'NONE',  ( 16.55507374853184999, 19.21127112649115531, 5.746835883940462963 ) ) ;
#14374 = CARTESIAN_POINT ( 'NONE',  ( 1.999999999999998224, -28.00000000000000000, 12.46410161513774639 ) ) ;
#14375 = ORIENTED_EDGE ( 'NONE', *, *, #23354, .T. ) ;
#14376 = CARTESIAN_POINT ( 'NONE',  ( 4.000000000000001776, 27.15624999877097423, 11.30940107675849760 ) ) ;
#14377 = CARTESIAN_POINT ( 'NONE',  ( 4.000000000000003553, 26.74374999877096926, 8.999999999999992895 ) ) ;
#14378 = CARTESIAN_POINT ( 'NONE',  ( -3.756430356250004099, -27.42812499938548143, 6.831223922626973533 ) ) ;
#14380 = ORIENTED_EDGE ( 'NONE', *, *, #4312, .F. ) ;
#14379 = CARTESIAN_POINT ( 'NONE',  ( 3.369928719974892281E-15, 25.11250000000000426, 4.999999999999992006 ) ) ;
#14381 = EDGE_CURVE ( 'NONE', #7537, #7733, #18628, .T. ) ;
#14382 = ORIENTED_EDGE ( 'NONE', *, *, #3335, .T. ) ;
#14383 = CARTESIAN_POINT ( 'NONE',  ( -3.756430356250003655, -25.14062499938548356, 8.999999999999992895 ) ) ;
#14384 = ORIENTED_EDGE ( 'NONE', *, *, #16031, .T. ) ;
#14385 = ORIENTED_EDGE ( 'NONE', *, *, #12577, .F. ) ;
#14386 =( NAMED_UNIT ( * ) PLANE_ANGLE_UNIT ( ) SI_UNIT ( $, .RADIAN. ) );
#14387 = CARTESIAN_POINT ( 'NONE',  ( 1.878215178125001605, 26.52812499938548640, 12.25316411605952283 ) ) ;
#14388 = CARTESIAN_POINT ( 'NONE',  ( 3.469446951953614189E-15, 25.00000000000000000, 8.999999999999992895 ) ) ;
#14389 =( BOUNDED_CURVE ( )  B_SPLINE_CURVE ( 2, ( #17784, #25499, #13605, #21571, #1956, #15573, #8544, #23541, #9804 ),
 .UNSPECIFIED., .F., .F. ) 
 B_SPLINE_CURVE_WITH_KNOTS ( ( 3, 2, 2, 2, 3 ),
 ( 0.5750000000000000666, 0.5833333333333333703, 0.5999999999999999778, 0.6166666666666666963, 0.6250000000000000000 ),
 .UNSPECIFIED. ) 
 CURVE ( )  GEOMETRIC_REPRESENTATION_ITEM ( )  RATIONAL_B_SPLINE_CURVE ( ( 0.9330127018922194093, 0.9330127018922198534, 1.000000000000000000, 0.8660254037844387076, 1.000000000000000000, 0.8660254037844387076, 1.000000000000000000, 0.9330127018922194093, 0.9330127018922194093 ) ) 
 REPRESENTATION_ITEM ( '' )  );
#14390 = FACE_OUTER_BOUND ( 'NONE', #18611, .T. ) ;
#14391 = CARTESIAN_POINT ( 'NONE',  ( -3.756430356249997882, -11.16877607737301226, 2.315624999385482496 ) ) ;
#14392 = CARTESIAN_POINT ( 'NONE',  ( 2.672651547586948120E-15, 25.47812499938548569, 13.33755215474602984 ) ) ;
#14393 = CARTESIAN_POINT ( 'NONE',  ( -27.00874656207317059, -15.41874213889385459, -2.750000000000000000 ) ) ;
#14394 = FACE_OUTER_BOUND ( 'NONE', #10849, .T. ) ;
#14395 = CARTESIAN_POINT ( 'NONE',  ( 2.672651547586948120E-15, 26.37812499938548427, 13.33755215474603162 ) ) ;
#14396 = CARTESIAN_POINT ( 'NONE',  ( -1.499999999999998224, -7.499999999999992895, 30.00000000000000355 ) ) ;
#14397 = DIRECTION ( 'NONE',  ( 0.000000000000000000, 0.000000000000000000, 1.000000000000000000 ) ) ;
#14398 = FACE_OUTER_BOUND ( 'NONE', #2221, .T. ) ;
#14399 = CARTESIAN_POINT ( 'NONE',  ( 3.999999999999997335, -28.35624999877096997, 11.30940107675849404 ) ) ;
#14400 = CARTESIAN_POINT ( 'NONE',  ( -1.071796769724481901, 28.01740381056766438, 12.99999999999999645 ) ) ;
#14401 = CYLINDRICAL_SURFACE ( 'NONE', #21670, 31.10000000000000142 ) ;
#14402 = CARTESIAN_POINT ( 'NONE',  ( -25.98730014090418194, 17.08421000182805471, -6.500000000000000000 ) ) ;
#14403 = EDGE_CURVE ( 'NONE', #19826, #19523, #1189, .T. ) ;
#14404 = VERTEX_POINT ( 'NONE', #4918 ) ;
#14405 = CARTESIAN_POINT ( 'NONE',  ( 0.7500000000000001110, 0.000000000000000000, 15.00000000000000178 ) ) ;
#14407 = VERTEX_POINT ( 'NONE', #19041 ) ;
#14406 = DIRECTION ( 'NONE',  ( 0.000000000000000000, 1.000000000000000000, 0.000000000000000000 ) ) ;
#14408 = ORIENTED_EDGE ( 'NONE', *, *, #11265, .T. ) ;
#14409 = ORIENTED_EDGE ( 'NONE', *, *, #14768, .F. ) ;
#14410 = EDGE_LOOP ( 'NONE', ( #19704, #6153, #19054, #7801 ) ) ;
#14411 = ORIENTED_EDGE ( 'NONE', *, *, #21469, .T. ) ;
#14412 = ORIENTED_EDGE ( 'NONE', *, *, #9364, .T. ) ;
#14413 = CARTESIAN_POINT ( 'NONE',  ( 0.000000000000000000, 0.000000000000000000, -6.500000000000000000 ) ) ;
#14414 = EDGE_CURVE ( 'NONE', #17868, #6671, #9144, .T. ) ;
#14415 = ORIENTED_EDGE ( 'NONE', *, *, #13233, .F. ) ;
#14416 = FACE_OUTER_BOUND ( 'NONE', #14022, .T. ) ;
#14417 = CARTESIAN_POINT ( 'NONE',  ( -1.878215178124998497, 26.00312499938548783, 12.25316411605951927 ) ) ;
#14418 = AXIS2_PLACEMENT_3D ( 'NONE', #7382, #19410, #25183 ) ;
#14419 = CARTESIAN_POINT ( 'NONE',  ( -1.878215178124998497, -12.25316411605951927, 3.703124999385482674 ) ) ;
#14420 = CARTESIAN_POINT ( 'NONE',  ( -23.96296185032681336, 19.82388608118453632, 1.000000000000000000 ) ) ;
#14421 = CARTESIAN_POINT ( 'NONE',  ( 21.09621640565530853, 15.78382164973649537, 6.831223922626973533 ) ) ;
#14422 = CARTESIAN_POINT ( 'NONE',  ( -25.99519186311192342, -0.5000000000000000000, 19.00000000000000000 ) ) ;
#14423 = CARTESIAN_POINT ( 'NONE',  ( -3.756430356249996994, -8.999999999999992895, 2.165624999385482141 ) ) ;
#14424 = CARTESIAN_POINT ( 'NONE',  ( 4.000000000000003553, -8.999999999999992895, 4.500000000000000888 ) ) ;
#14425 = CARTESIAN_POINT ( 'NONE',  ( -29.62293631110050995, -7.734255490826679846, -6.500000000000000000 ) ) ;
#14426 = CARTESIAN_POINT ( 'NONE',  ( 1.878215178125000939, 29.11562499938548498, 12.25316411605952283 ) ) ;
#14427 = CARTESIAN_POINT ( 'NONE',  ( -1.878215178124995832, -5.746835883940462963, 3.103124999385483029 ) ) ;
#14428 = CARTESIAN_POINT ( 'NONE',  ( -24.27856662945521649, -19.43607991388963185, -6.500000000000000000 ) ) ;
#14429 = DIRECTION ( 'NONE',  ( 0.000000000000000000, 0.000000000000000000, -1.000000000000000000 ) ) ;
#14430 = ORIENTED_EDGE ( 'NONE', *, *, #10638, .T. ) ;
#14431 = ORIENTED_EDGE ( 'NONE', *, *, #3960, .F. ) ;
#14432 = CARTESIAN_POINT ( 'NONE',  ( 1.878215178125005158, 28.47812499938549280, 5.746835883940462963 ) ) ;
#14433 =( BOUNDED_CURVE ( )  B_SPLINE_CURVE ( 2, ( #24453, #10704, #400, #4183, #6531, #660, #8369, #14647, #778 ),
 .UNSPECIFIED., .F., .F. ) 
 B_SPLINE_CURVE_WITH_KNOTS ( ( 3, 2, 2, 2, 3 ),
 ( 0.7249999999999999778, 0.7333333333333332815, 0.7500000000000000000, 0.7666666666666667185, 0.7750000000000000222 ),
 .UNSPECIFIED. ) 
 CURVE ( )  GEOMETRIC_REPRESENTATION_ITEM ( )  RATIONAL_B_SPLINE_CURVE ( ( 0.9330127018922194093, 0.9330127018922194093, 1.000000000000000000, 0.8660254037844387076, 1.000000000000000000, 0.8660254037844387076, 1.000000000000000000, 0.9330127018922194093, 0.9330127018922194093 ) ) 
 REPRESENTATION_ITEM ( '' )  );
#14434 = EDGE_CURVE ( 'NONE', #22312, #11375, #20482, .T. ) ;
#14435 = ORIENTED_EDGE ( 'NONE', *, *, #19056, .T. ) ;
#14436 = CARTESIAN_POINT ( 'NONE',  ( 4.000000000000003553, 25.03750000000000142, 6.690598923241489970 ) ) ;
#14437 = ORIENTED_EDGE ( 'NONE', *, *, #6426, .T. ) ;
#14438 = CARTESIAN_POINT ( 'NONE',  ( -1.071796769724487230, 26.03259618943233278, 4.999999999999992006 ) ) ;
#14439 = EDGE_CURVE ( 'NONE', #3560, #21567, #19141, .T. ) ;
#14440 = ORIENTED_EDGE ( 'NONE', *, *, #13263, .F. ) ;
#14441 = DIRECTION ( 'NONE',  ( 1.000000000000000000, 0.000000000000000000, 0.000000000000000000 ) ) ;
#14442 = DIRECTION ( 'NONE',  ( -0.8443279255020122998, 0.5358267949790012086, 0.000000000000000000 ) ) ;
#14443 = ORIENTED_EDGE ( 'NONE', *, *, #4253, .T. ) ;
#14444 = ADVANCED_FACE ( 'NONE', ( #25202, #11705 ), #7661, .T. ) ;
#14445 = B_SPLINE_CURVE_WITH_KNOTS ( 'NONE', 3,
 ( #1557, #5611, #18039, #15943, #13847, #11993, #13592, #124, #21686, #15804, #25486, #15683, #17893, #19846, #21559, #23651 ),
 .UNSPECIFIED., .F., .F.,
 ( 4, 2, 2, 2, 2, 2, 2, 4 ),
 ( 2.789812634829633135E-07, 0.0002322844908106884518, 0.0004642900003578939055, 0.0006962955099050993591, 0.0009283010194523048670, 0.001160306528999510483, 0.001392312038546715883, 0.001856323057641126898 ),
 .UNSPECIFIED. ) ;
#14446 = CARTESIAN_POINT ( 'NONE',  ( 3.834746474454188013E-15, 28.65624999877096712, 4.999999999999992006 ) ) ;
#14447 = CARTESIAN_POINT ( 'NONE',  ( 3.756430356250004099, 26.97812499938548569, 6.831223922626973533 ) ) ;
#14448 = DIRECTION ( 'NONE',  ( 0.000000000000000000, 0.000000000000000000, -1.000000000000000000 ) ) ;
#14449 = CARTESIAN_POINT ( 'NONE',  ( 2.000000000000000888, 26.72500000000000142, 12.46410161513774817 ) ) ;
#14450 = LINE ( 'NONE', #23991, #24620 ) ;
#14451 = CARTESIAN_POINT ( 'NONE',  ( 8.012344526598182026E-15, 28.71250000000000568, 4.381197846482986158 ) ) ;
#14452 = AXIS2_PLACEMENT_3D ( 'NONE', #14558, #5239, #15436 ) ;
#14453 = CARTESIAN_POINT ( 'NONE',  ( 1.878215178125000939, 26.86562499938548498, 12.25316411605952283 ) ) ;
#14454 = CARTESIAN_POINT ( 'NONE',  ( -1.999999999999995781, 26.05000000000000071, 5.535898384862237620 ) ) ;
#14455 = CARTESIAN_POINT ( 'NONE',  ( 21.58443449571939965, 18.75600737097314052, 12.46410161513774817 ) ) ;
#14456 = DIRECTION ( 'NONE',  ( -0.000000000000000000, -1.000000000000000000, 0.000000000000000000 ) ) ;
#14457 = CARTESIAN_POINT ( 'NONE',  ( -1.057460391440397258E-14, 29.10624999877096641, 4.999999999999992006 ) ) ;
#14458 = CARTESIAN_POINT ( 'NONE',  ( -3.756430356250003211, -26.07812499938548356, 6.831223922626973533 ) ) ;
#14459 = CARTESIAN_POINT ( 'NONE',  ( 23.01025686871630782, -20.92219106202058754, 1.000000000000000000 ) ) ;
#14460 = VERTEX_POINT ( 'NONE', #25317 ) ;
#14461 = CARTESIAN_POINT ( 'NONE',  ( -1.878215178124998497, 26.00312499938548783, 12.25316411605951927 ) ) ;
#14462 = CARTESIAN_POINT ( 'NONE',  ( 3.999999999999997335, -27.96250000000000213, 11.30940107675849404 ) ) ;
#14464 = ORIENTED_EDGE ( 'NONE', *, *, #20276, .F. ) ;
#14463 = CARTESIAN_POINT ( 'NONE',  ( -3.756430356249994773, 28.17812499938548854, 8.999999999999992895 ) ) ;
#14465 = ORIENTED_EDGE ( 'NONE', *, *, #12347, .F. ) ;
#14466 = FACE_OUTER_BOUND ( 'NONE', #17066, .T. ) ;
#14467 = CARTESIAN_POINT ( 'NONE',  ( -3.999999999999995559, 25.58124999877096784, 6.690598923241487306 ) ) ;
#14468 = EDGE_LOOP ( 'NONE', ( #1599, #24548, #25720, #20894, #4786, #4118 ) ) ;
#14469 = EDGE_LOOP ( 'NONE', ( #25385, #23977, #7027, #21240 ) ) ;
#14470 = EDGE_CURVE ( 'NONE', #17209, #7506, #1593, .T. ) ;
#14471 = CARTESIAN_POINT ( 'NONE',  ( -1.878215178125004048, -26.67812499938548498, 5.746835883940462963 ) ) ;
#14472 = CARTESIAN_POINT ( 'NONE',  ( 3.756430356250002323, 27.42812499938548498, 6.831223922626973533 ) ) ;
#14473 = CARTESIAN_POINT ( 'NONE',  ( 19.30843454290614147, 19.30843454290607752, 4.999999999999991118 ) ) ;
#14474 = EDGE_CURVE ( 'NONE', #8943, #3881, #17230, .T. ) ;
#14475 = DIRECTION ( 'NONE',  ( -0.000000000000000000, -0.000000000000000000, 1.000000000000000000 ) ) ;
#14476 = DIRECTION ( 'NONE',  ( -0.000000000000000000, 1.000000000000000000, 0.000000000000000000 ) ) ;
#14477 = DIRECTION ( 'NONE',  ( 0.000000000000000000, 0.000000000000000000, -1.000000000000000000 ) ) ;
#14478 = CARTESIAN_POINT ( 'NONE',  ( -20.92219106202016476, 23.01025686871669507, -6.500000000000000000 ) ) ;
#14479 = CARTESIAN_POINT ( 'NONE',  ( 0.000000000000000000, 0.000000000000000000, -6.500000000000000000 ) ) ;
#14480 = CARTESIAN_POINT ( 'NONE',  ( 0.000000000000000000, 0.000000000000000000, 1.000000000000000000 ) ) ;
#14481 = CARTESIAN_POINT ( 'NONE',  ( 19.28854716511979461, 19.28854716511973066, 13.33755215474602984 ) ) ;
#14482 = CARTESIAN_POINT ( 'NONE',  ( 19.14933551713916771, 19.14933551713910020, 13.61880215351699874 ) ) ;
#14483 = CARTESIAN_POINT ( 'NONE',  ( 4.000000000000003553, 27.73750000000000071, 6.690598923241489970 ) ) ;
#14484 = CARTESIAN_POINT ( 'NONE',  ( 22.22083059878729117, 19.39240347404102849, 12.46410161513774817 ) ) ;
#14485 = CARTESIAN_POINT ( 'NONE',  ( 3.735045420075836212E-15, 26.15312499938548285, 4.662447845253954171 ) ) ;
#14487 = VERTEX_POINT ( 'NONE', #1516 ) ;
#14486 = LINE ( 'NONE', #14370, #7457 ) ;
#14488 = CARTESIAN_POINT ( 'NONE',  ( 20.45982030258741702, 15.14742554666860563, 6.831223922626973533 ) ) ;
#14489 = DIRECTION ( 'NONE',  ( 0.000000000000000000, 0.000000000000000000, 1.000000000000000000 ) ) ;
#14490 = ORIENTED_EDGE ( 'NONE', *, *, #3230, .T. ) ;
#14491 = CARTESIAN_POINT ( 'NONE',  ( -3.999999999999996447, -8.999999999999992895, 18.00000000000000000 ) ) ;
#14492 = DIRECTION ( 'NONE',  ( 1.000000000000000000, 0.000000000000000000, 0.000000000000000000 ) ) ;
#14493 = CARTESIAN_POINT ( 'NONE',  ( -3.735045420075836212E-15, -26.60312499938547859, 4.662447845253954171 ) ) ;
#14495 = ORIENTED_EDGE ( 'NONE', *, *, #8949, .F. ) ;
#14494 = CARTESIAN_POINT ( 'NONE',  ( 4.000000000000003553, -8.999999999999992895, 18.00000000000000000 ) ) ;
#14496 = CARTESIAN_POINT ( 'NONE',  ( 2.000000000000000000, 29.81874999877097210, 12.46410161513774817 ) ) ;
#14497 = ORIENTED_EDGE ( 'NONE', *, *, #18566, .T. ) ;
#14498 = EDGE_CURVE ( 'NONE', #2175, #14315, #13428, .T. ) ;
#14499 = CARTESIAN_POINT ( 'NONE',  ( -3.756430356250003655, -29.75312499938548783, 8.999999999999992895 ) ) ;
#14500 = VERTEX_POINT ( 'NONE', #3343 ) ;
#14501 = ORIENTED_EDGE ( 'NONE', *, *, #13959, .F. ) ;
#14502 = FACE_OUTER_BOUND ( 'NONE', #24310, .T. ) ;
#14503 = EDGE_CURVE ( 'NONE', #990, #6938, #4702, .T. ) ;
#14504 = DIRECTION ( 'NONE',  ( 0.000000000000000000, 1.000000000000000000, 0.000000000000000000 ) ) ;
#14505 = CARTESIAN_POINT ( 'NONE',  ( 3.756430356250002323, -11.16877607737301226, 1.115624999385483429 ) ) ;
#14506 = DIRECTION ( 'NONE',  ( 0.000000000000000000, 0.000000000000000000, 1.000000000000000000 ) ) ;
#14507 = CARTESIAN_POINT ( 'NONE',  ( 3.756430356250004099, 25.17812499938548498, 6.831223922626973533 ) ) ;
#14508 = EDGE_CURVE ( 'NONE', #9980, #16142, #19977, .T. ) ;
#14509 = DIRECTION ( 'NONE',  ( -0.000000000000000000, -1.000000000000000000, -0.000000000000000000 ) ) ;
#14510 = DIRECTION ( 'NONE',  ( 0.000000000000000000, -0.000000000000000000, 1.000000000000000000 ) ) ;
#14511 = CARTESIAN_POINT ( 'NONE',  ( 3.756430356250003655, 25.59062499938548285, 8.999999999999992895 ) ) ;
#14512 = CARTESIAN_POINT ( 'NONE',  ( 0.000000000000000000, 0.000000000000000000, -6.500000000000000000 ) ) ;
#14513 = FACE_OUTER_BOUND ( 'NONE', #24095, .T. ) ;
#14514 = CARTESIAN_POINT ( 'NONE',  ( -27.00874656207317059, -15.41874213889385459, -6.500000000000000000 ) ) ;
#14515 = CARTESIAN_POINT ( 'NONE',  ( 1.878215178124998497, -26.90312499938548285, 12.25316411605951927 ) ) ;
#14516 = CARTESIAN_POINT ( 'NONE',  ( -1.999999999999998224, 27.55000000000000426, 12.46410161513774639 ) ) ;
#14517 = DIRECTION ( 'NONE',  ( 3.552713678800501718E-15, 0.000000000000000000, 1.000000000000000000 ) ) ;
#14518 = DIRECTION ( 'NONE',  ( 0.000000000000000000, 0.000000000000000000, 1.000000000000000000 ) ) ;
#14519 = DIRECTION ( 'NONE',  ( 0.000000000000000000, 1.000000000000000000, 0.000000000000000000 ) ) ;
#14520 = VERTEX_POINT ( 'NONE', #9371 ) ;
#14521 = CARTESIAN_POINT ( 'NONE',  ( 4.000000000000002665, 27.60624999877096641, 11.30940107675849760 ) ) ;
#14523 = VERTEX_POINT ( 'NONE', #11452 ) ;
#14522 = FACE_OUTER_BOUND ( 'NONE', #14137, .T. ) ;
#14524 = VERTEX_POINT ( 'NONE', #11570 ) ;
#14525 = EDGE_LOOP ( 'NONE', ( #6359, #4457, #6424, #994 ) ) ;
#14526 = VERTEX_POINT ( 'NONE', #17352 ) ;
#14527 = ORIENTED_EDGE ( 'NONE', *, *, #2082, .T. ) ;
#14528 = VERTEX_POINT ( 'NONE', #23348 ) ;
#14529 = CARTESIAN_POINT ( 'NONE',  ( 0.7500000000000000000, -2.999999999999999556, 17.69999999999999929 ) ) ;
#14530 = EDGE_LOOP ( 'NONE', ( #1134, #22918, #2183, #23563 ) ) ;
#14531 = FACE_OUTER_BOUND ( 'NONE', #15537, .T. ) ;
#14532 = CARTESIAN_POINT ( 'NONE',  ( 3.735045420075836212E-15, 28.51562499938548356, 4.662447845253954171 ) ) ;
#14533 = EDGE_CURVE ( 'NONE', #17574, #11405, #5437, .T. ) ;
#14534 = CARTESIAN_POINT ( 'NONE',  ( 3.756430356250002323, -11.16877607737301226, 2.915624999385482141 ) ) ;
#14535 = SURFACE_STYLE_USAGE ( .BOTH. , #18474 ) ;
#14536 = CARTESIAN_POINT ( 'NONE',  ( 16.57931677857143882, 21.89171153449011697, 11.16877607737301226 ) ) ;
#14537 = CYLINDRICAL_SURFACE ( 'NONE', #15501, 4.000000000000000000 ) ;
#14538 = DIRECTION ( 'NONE',  ( -0.000000000000000000, -0.000000000000000000, 1.000000000000000000 ) ) ;
#14539 = CIRCLE ( 'NONE', #8268, 3.000000000000000444 ) ;
#14540 = CARTESIAN_POINT ( 'NONE',  ( 2.672651547586948120E-15, -13.33755215474602984, 1.378124999385482274 ) ) ;
#14541 = CARTESIAN_POINT ( 'NONE',  ( -28.14012133169333651, -13.24173596767349359, 1.000000000000000000 ) ) ;
#14542 = CARTESIAN_POINT ( 'NONE',  ( 4.000000000000001776, -11.30940107675849760, 4.012499999999996625 ) ) ;
#14543 = CARTESIAN_POINT ( 'NONE',  ( 4.143002691484658293E-15, 39.50000000000000000, 13.99999999999999289 ) ) ;
#14544 = CARTESIAN_POINT ( 'NONE',  ( 1.878215178125004048, 28.81562499938548427, 5.746835883940462963 ) ) ;
#14545 = CARTESIAN_POINT ( 'NONE',  ( -3.756430356249996994, -8.999999999999992895, 1.378124999385485605 ) ) ;
#14546 = CARTESIAN_POINT ( 'NONE',  ( -2.000000000000003997, -28.22500000000000142, 5.535898384862238508 ) ) ;
#14547 = AXIS2_PLACEMENT_3D ( 'NONE', #14267, #3932, #14003 ) ;
#14548 = ORIENTED_EDGE ( 'NONE', *, *, #12980, .F. ) ;
#14549 = ORIENTED_EDGE ( 'NONE', *, *, #5541, .T. ) ;
#14550 = CARTESIAN_POINT ( 'NONE',  ( -1.878215178124998275, 27.35312499938548925, 12.25316411605951927 ) ) ;
#14551 = EDGE_LOOP ( 'NONE', ( #14078, #14385, #16081, #15469 ) ) ;
#14552 = CARTESIAN_POINT ( 'NONE',  ( -21.28941499438242246, -22.67092431280570963, -6.500000000000000000 ) ) ;
#14553 = ORIENTED_EDGE ( 'NONE', *, *, #13804, .F. ) ;
#14554 = DIRECTION ( 'NONE',  ( 0.000000000000000000, -1.000000000000000000, 0.000000000000000000 ) ) ;
#14555 = ORIENTED_EDGE ( 'NONE', *, *, #3162, .T. ) ;
#14556 = CARTESIAN_POINT ( 'NONE',  ( -3.469446951953614189E-15, -30.00000000000000355, 4.999999999999992006 ) ) ;
#14557 = VECTOR ( 'NONE', #5195, 1000.000000000000000 ) ;
#14558 = CARTESIAN_POINT ( 'NONE',  ( -30.85476721088030061, -3.897863563849544466, -6.500000000000000000 ) ) ;
#14559 = VERTEX_POINT ( 'NONE', #3723 ) ;
#14560 = AXIS2_PLACEMENT_3D ( 'NONE', #16180, #20225, #13837 ) ;
#14561 = DIRECTION ( 'NONE',  ( 1.000000000000000000, 0.000000000000000000, 0.000000000000000000 ) ) ;
#14562 = CARTESIAN_POINT ( 'NONE',  ( 2.672651547586948120E-15, 29.07812499938548001, 13.33755215474602984 ) ) ;
#14563 = DIRECTION ( 'NONE',  ( 1.000000000000000000, 0.000000000000000000, 0.000000000000000000 ) ) ;
#14564 = EDGE_CURVE ( 'NONE', #23529, #22370, #25060, .T. ) ;
#14565 = VECTOR ( 'NONE', #5604, 1000.000000000000000 ) ;
#14566 = CARTESIAN_POINT ( 'NONE',  ( 21.65113613650343538, 22.32573188046912449, -6.500000000000000000 ) ) ;
#14567 = CARTESIAN_POINT ( 'NONE',  ( 0.000000000000000000, 0.000000000000000000, 20.00000000000000000 ) ) ;
#14568 = CARTESIAN_POINT ( 'NONE',  ( -1.999999999999998224, 28.90000000000000924, 12.46410161513774639 ) ) ;
#14569 = EDGE_CURVE ( 'NONE', #11941, #16614, #7149, .T. ) ;
#14570 = CARTESIAN_POINT ( 'NONE',  ( 1.878215178125004048, 27.01562499938548711, 5.746835883940462963 ) ) ;
#14571 = EDGE_CURVE ( 'NONE', #20492, #24486, #14988, .T. ) ;
#14572 =( BOUNDED_CURVE ( )  B_SPLINE_CURVE ( 2, ( #18583, #16498, #20267, #14521, #18837, #24462, #409, #18316, #2750 ),
 .UNSPECIFIED., .F., .F. ) 
 B_SPLINE_CURVE_WITH_KNOTS ( ( 3, 2, 2, 2, 3 ),
 ( 0.4750000000000000333, 0.4833333333333333370, 0.5000000000000000000, 0.5166666666666667185, 0.5250000000000000222 ),
 .UNSPECIFIED. ) 
 CURVE ( )  GEOMETRIC_REPRESENTATION_ITEM ( )  RATIONAL_B_SPLINE_CURVE ( ( 0.9330127018922194093, 0.9330127018922196314, 1.000000000000000000, 0.8660254037844387076, 1.000000000000000000, 0.8660254037844387076, 1.000000000000000000, 0.9330127018922194093, 0.9330127018922194093 ) ) 
 REPRESENTATION_ITEM ( '' )  );
#14573 = CARTESIAN_POINT ( 'NONE',  ( 20.83105136271035462, 15.51865660679153969, 8.999999999999992895 ) ) ;
#14574 = CIRCLE ( 'NONE', #3295, 0.5000000000000011102 ) ;
#14575 = AXIS2_PLACEMENT_3D ( 'NONE', #16318, #19835, #4017 ) ;
#14576 = CARTESIAN_POINT ( 'NONE',  ( 20.46190248058575634, 20.46190248058568528, 13.61880215351699874 ) ) ;
#14577 = EDGE_CURVE ( 'NONE', #23624, #17423, #23326, .T. ) ;
#14578 = CARTESIAN_POINT ( 'NONE',  ( 1.859271017917182139E-15, 29.38749999999999929, 12.99999999999999289 ) ) ;
#14579 = CARTESIAN_POINT ( 'NONE',  ( 3.999999999999995559, -27.83124999877096784, 6.690598923241487306 ) ) ;
#14580 = CARTESIAN_POINT ( 'NONE',  ( 3.756430356249996994, -26.26562499938548711, 8.999999999999992895 ) ) ;
#14581 = CARTESIAN_POINT ( 'NONE',  ( 0.000000000000000000, 0.000000000000000000, 1.000000000000000000 ) ) ;
#14582 = VERTEX_POINT ( 'NONE', #23870 ) ;
#14583 = CARTESIAN_POINT ( 'NONE',  ( 4.000000000000003553, 29.44374999877096855, 8.999999999999992895 ) ) ;
#14584 = CARTESIAN_POINT ( 'NONE',  ( 3.999999999999996003, -28.33750000000000213, 6.690598923241487306 ) ) ;
#14586 = ORIENTED_EDGE ( 'NONE', *, *, #9092, .T. ) ;
#14585 = CARTESIAN_POINT ( 'NONE',  ( 3.756430356250004099, 29.71562499938548996, 11.16877607737301403 ) ) ;
#14587 = ORIENTED_EDGE ( 'NONE', *, *, #12188, .T. ) ;
#14588 = DIRECTION ( 'NONE',  ( 1.000000000000000000, 0.000000000000000000, 0.000000000000000000 ) ) ;
#14589 = FACE_OUTER_BOUND ( 'NONE', #1172, .T. ) ;
#14590 = VERTEX_POINT ( 'NONE', #9870 ) ;
#14591 = CARTESIAN_POINT ( 'NONE',  ( 3.756430356249997438, -25.96562499938548640, 11.16877607737301048 ) ) ;
#14592 = CARTESIAN_POINT ( 'NONE',  ( 4.006172263299091013E-15, 28.17812499938548498, 13.33755215474602984 ) ) ;
#14593 = CARTESIAN_POINT ( 'NONE',  ( -0.5000000000000000000, 0.8660254037844387076, 20.00000000000000000 ) ) ;
#14594 = AXIS2_PLACEMENT_3D ( 'NONE', #24024, #11734, #14087 ) ;
#14595 = CIRCLE ( 'NONE', #10829, 0.4999999999999999445 ) ;
#14596 = CARTESIAN_POINT ( 'NONE',  ( -30.54913349766215802, 5.827558883616378083, -6.500000000000000000 ) ) ;
#14597 = CARTESIAN_POINT ( 'NONE',  ( -3.756430356249996105, 25.77812499938548640, 6.831223922626973533 ) ) ;
#14598 = VECTOR ( 'NONE', #14056, 1000.000000000000000 ) ;
#14599 = CIRCLE ( 'NONE', #24621, 0.4999999999999998890 ) ;
#14600 = DIRECTION ( 'NONE',  ( -0.000000000000000000, -1.000000000000000000, -0.000000000000000000 ) ) ;
#14601 = DIRECTION ( 'NONE',  ( -1.000000000000000000, 0.000000000000000000, 0.000000000000000000 ) ) ;
#14602 = ADVANCED_FACE ( 'NONE', ( #5955 ), #19808, .F. ) ;
#14603 = DIRECTION ( 'NONE',  ( 0.000000000000000000, 0.000000000000000000, 1.000000000000000000 ) ) ;
#14604 = DIRECTION ( 'NONE',  ( -0.000000000000000000, -0.000000000000000000, 1.000000000000000000 ) ) ;
#14605 = LINE ( 'NONE', #18401, #14677 ) ;
#14606 = AXIS2_PLACEMENT_3D ( 'NONE', #1344, #17171, #23565 ) ;
#14607 = DIRECTION ( 'NONE',  ( 0.000000000000000000, 0.000000000000000000, 1.000000000000000000 ) ) ;
#14608 = CARTESIAN_POINT ( 'NONE',  ( 22.31597560320210505, 17.00358084728328478, 11.16877607737301226 ) ) ;
#14609 = CARTESIAN_POINT ( 'NONE',  ( 23.33010436090463102, 17.67325011141217317, 8.999999999999992895 ) ) ;
#14610 = EDGE_CURVE ( 'NONE', #21069, #20277, #21237, .T. ) ;
#14611 = CARTESIAN_POINT ( 'NONE',  ( -3.999999999999997335, 28.41250000000000142, 11.30940107675849404 ) ) ;
#14612 = LINE ( 'NONE', #24812, #19258 ) ;
#14613 = CARTESIAN_POINT ( 'NONE',  ( 1.878215178125000939, 26.41562499938548214, 12.25316411605952283 ) ) ;
#14614 = EDGE_CURVE ( 'NONE', #23568, #10460, #15399, .T. ) ;
#14616 = ORIENTED_EDGE ( 'NONE', *, *, #3265, .F. ) ;
#14615 = DIRECTION ( 'NONE',  ( 0.3090169943749591086, 0.9510565162951497564, 0.000000000000000000 ) ) ;
#14617 = VECTOR ( 'NONE', #16977, 1000.000000000000000 ) ;
#14618 = CARTESIAN_POINT ( 'NONE',  ( -30.35476721088030061, -3.897863563849544466, -6.500000000000000000 ) ) ;
#14619 = DIRECTION ( 'NONE',  ( 1.000000000000000000, 0.000000000000000000, 0.000000000000000000 ) ) ;
#14620 = ORIENTED_EDGE ( 'NONE', *, *, #8296, .T. ) ;
#14621 = DIRECTION ( 'NONE',  ( 0.7289686274214236539, 0.6845471059286760696, 0.000000000000000000 ) ) ;
#14622 = CARTESIAN_POINT ( 'NONE',  ( 2.000000000000003997, 28.16874999877096997, 5.535898384862238508 ) ) ;
#14623 = CARTESIAN_POINT ( 'NONE',  ( 3.756430356249995661, -27.57812499938548356, 6.831223922626973533 ) ) ;
#14625 = ORIENTED_EDGE ( 'NONE', *, *, #12468, .T. ) ;
#14624 = CARTESIAN_POINT ( 'NONE',  ( 0.000000000000000000, 0.000000000000000000, -6.500000000000000000 ) ) ;
#14626 = DIRECTION ( 'NONE',  ( -0.000000000000000000, -0.000000000000000000, 1.000000000000000000 ) ) ;
#14627 = VECTOR ( 'NONE', #15858, 1000.000000000000000 ) ;
#14628 = EDGE_LOOP ( 'NONE', ( #19885, #13923, #21209, #25391 ) ) ;
#14629 = CARTESIAN_POINT ( 'NONE',  ( 1.878215178124995832, -25.74062499938548498, 5.746835883940462963 ) ) ;
#14630 = ORIENTED_EDGE ( 'NONE', *, *, #25697, .T. ) ;
#14631 = VERTEX_POINT ( 'NONE', #17854 ) ;
#14632 = DIRECTION ( 'NONE',  ( 0.000000000000000000, 0.000000000000000000, 1.000000000000000000 ) ) ;
#14633 = CARTESIAN_POINT ( 'NONE',  ( -1.071796769724488563, 27.06115380933863435, 12.99999999999999289 ) ) ;
#14634 = CARTESIAN_POINT ( 'NONE',  ( -3.999999999999966249, -11.30940107675851181, 3.356249998770968190 ) ) ;
#14635 = AXIS2_PLACEMENT_3D ( 'NONE', #13875, #3931, #1580 ) ;
#14636 = AXIS2_PLACEMENT_3D ( 'NONE', #7112, #5159, #13136 ) ;
#14637 = CARTESIAN_POINT ( 'NONE',  ( -1.878215178124998497, -12.25316411605951927, 2.353124999385485694 ) ) ;
#14638 =( NAMED_UNIT ( * ) PLANE_ANGLE_UNIT ( ) SI_UNIT ( $, .RADIAN. ) );
#14639 = CLOSED_SHELL ( 'NONE', ( #4936, #19694, #3309, #20551, #4710, #11084, #11022, #1471, #14819, #19714, #24870, #24317 ) ) ;
#14640 = CARTESIAN_POINT ( 'NONE',  ( -3.068646161593051591, 38.57519691277454399, 3.931793986884403402 ) ) ;
#14641 = CARTESIAN_POINT ( 'NONE',  ( -3.756430356249997882, 29.56562499938549138, 11.16877607737301226 ) ) ;
#14642 = CARTESIAN_POINT ( 'NONE',  ( 3.469446951953614189E-15, 38.49999999999999289, 8.999999999999992895 ) ) ;
#14643 = DIRECTION ( 'NONE',  ( 0.8763066800438685799, 0.4817536741017063306, 0.000000000000000000 ) ) ;
#14644 = CARTESIAN_POINT ( 'NONE',  ( 2.672651547586948120E-15, 27.72812499938548569, 13.33755215474603162 ) ) ;
#14645 = DIRECTION ( 'NONE',  ( 0.000000000000000000, 0.000000000000000000, 1.000000000000000000 ) ) ;
#14646 = LINE ( 'NONE', #22628, #12863 ) ;
#14647 = CARTESIAN_POINT ( 'NONE',  ( -1.071796769724488563, 28.86115380933863506, 12.99999999999999289 ) ) ;
#14648 = CARTESIAN_POINT ( 'NONE',  ( -2.672651547586948120E-15, -26.49062499938548143, 13.33755215474602984 ) ) ;
#14649 = LINE ( 'NONE', #2744, #5657 ) ;
#14650 = EDGE_CURVE ( 'NONE', #19628, #9493, #13940, .T. ) ;
#14651 = CARTESIAN_POINT ( 'NONE',  ( -3.999999999999995559, 27.88750000000000284, 6.690598923241487306 ) ) ;
#14652 = CIRCLE ( 'NONE', #6282, 0.4999999999999996669 ) ;
#14653 = CARTESIAN_POINT ( 'NONE',  ( 3.999999999999996447, -25.22500000000000142, 8.999999999999992895 ) ) ;
#14654 = CARTESIAN_POINT ( 'NONE',  ( -3.999999999999995559, 27.88750000000000284, 6.690598923241487306 ) ) ;
#14655 = EDGE_LOOP ( 'NONE', ( #2426, #23908, #17810, #16082 ) ) ;
#14656 = CARTESIAN_POINT ( 'NONE',  ( 0.5000000000000000000, 6.000000000000000000, 19.50000000000000000 ) ) ;
#14658 = ORIENTED_EDGE ( 'NONE', *, *, #21368, .F. ) ;
#14657 = LINE ( 'NONE', #18699, #9141 ) ;
#14659 = AXIS2_PLACEMENT_3D ( 'NONE', #272, #8240, #4438 ) ;
#14660 = ORIENTED_EDGE ( 'NONE', *, *, #18061, .F. ) ;
#14661 = ORIENTED_EDGE ( 'NONE', *, *, #8254, .F. ) ;
#14662 = ORIENTED_EDGE ( 'NONE', *, *, #5735, .T. ) ;
#14663 = VERTEX_POINT ( 'NONE', #3864 ) ;
#14664 = AXIS2_PLACEMENT_3D ( 'NONE', #18385, #16049, #2308 ) ;
#14665 = DIRECTION ( 'NONE',  ( 0.000000000000000000, 0.000000000000000000, 1.000000000000000000 ) ) ;
#14666 = AXIS2_PLACEMENT_3D ( 'NONE', #21844, #4045, #12289 ) ;
#14667 = VERTEX_POINT ( 'NONE', #13801 ) ;
#14668 = CYLINDRICAL_SURFACE ( 'NONE', #2749, 31.10000000000000142 ) ;
#14669 = CARTESIAN_POINT ( 'NONE',  ( 1.878215178125004048, 29.37812499938548783, 5.746835883940462963 ) ) ;
#14670 = AXIS2_PLACEMENT_3D ( 'NONE', #18238, #320, #4368 ) ;
#14671 = CARTESIAN_POINT ( 'NONE',  ( 1.878215178125004048, -5.746835883940462963, 2.128124999385486049 ) ) ;
#14672 = DIRECTION ( 'NONE',  ( -0.9921147013144768767, 0.1253332335643120576, 0.000000000000000000 ) ) ;
#14673 = PRODUCT_DEFINITION_SHAPE ( 'NONE', 'NONE',  #1360 ) ;
#14674 = CARTESIAN_POINT ( 'NONE',  ( 0.000000000000000000, 0.000000000000000000, 1.000000000000000000 ) ) ;
#14675 = CIRCLE ( 'NONE', #1722, 30.10000000000000142 ) ;
#14676 = LINE ( 'NONE', #8651, #14253 ) ;
#14677 = VECTOR ( 'NONE', #14362, 1000.000000000000000 ) ;
#14678 = CARTESIAN_POINT ( 'NONE',  ( 11.52193136556785369, -23.36965697125208052, 20.00001199999999457 ) ) ;
#14679 = CARTESIAN_POINT ( 'NONE',  ( 3.756430356250002323, -11.16877607737301226, 1.453124999385484228 ) ) ;
#14680 = DIRECTION ( 'NONE',  ( 0.000000000000000000, -0.000000000000000000, 1.000000000000000000 ) ) ;
#14681 = CARTESIAN_POINT ( 'NONE',  ( 2.000000000000000888, -12.46410161513774817, 3.075000000000001510 ) ) ;
#14682 = CARTESIAN_POINT ( 'NONE',  ( -1.999999999999993117, 28.69374999877097210, 5.535898384862237620 ) ) ;
#14683 = EDGE_CURVE ( 'NONE', #18554, #12515, #2028, .T. ) ;
#14684 = CARTESIAN_POINT ( 'NONE',  ( 1.071796769724487675, 29.14240381056766438, 4.999999999999988454 ) ) ;
#14685 = CIRCLE ( 'NONE', #6739, 31.10000000000000142 ) ;
#14686 = CARTESIAN_POINT ( 'NONE',  ( 3.756430356250002323, -11.16877607737301403, 2.915624999385482141 ) ) ;
#14687 = EDGE_CURVE ( 'NONE', #21027, #24856, #22810, .T. ) ;
#14688 = CARTESIAN_POINT ( 'NONE',  ( 3.469446951953614189E-15, -8.999999999999992895, 18.00000000000000000 ) ) ;
#14689 = CARTESIAN_POINT ( 'NONE',  ( 0.000000000000000000, 0.000000000000000000, 19.50000000000000000 ) ) ;
#14690 = VERTEX_POINT ( 'NONE', #7910 ) ;
#14691 = EDGE_LOOP ( 'NONE', ( #16497, #9498, #6065, #8840 ) ) ;
#14692 = CARTESIAN_POINT ( 'NONE',  ( -3.756430356249996105, 27.76562499938549422, 11.16877607737301226 ) ) ;
#14693 = EDGE_CURVE ( 'NONE', #24465, #1590, #9121, .T. ) ;
#14694 = VECTOR ( 'NONE', #18618, 1000.000000000000000 ) ;
#14695 = VERTEX_POINT ( 'NONE', #23997 ) ;
#14696 = CARTESIAN_POINT ( 'NONE',  ( -31.03863125411922752, 1.952785157361987878, 1.000000000000000000 ) ) ;
#14697 = ORIENTED_EDGE ( 'NONE', *, *, #8703, .F. ) ;
#14698 = CARTESIAN_POINT ( 'NONE',  ( -1.878215178125000939, -25.62812499938548783, 12.25316411605952283 ) ) ;
#14699 = ORIENTED_EDGE ( 'NONE', *, *, #330, .F. ) ;
#14700 = FACE_OUTER_BOUND ( 'NONE', #9358, .T. ) ;
#14701 = AXIS2_PLACEMENT_3D ( 'NONE', #21083, #17029, #20958 ) ;
#14702 = EDGE_CURVE ( 'NONE', #21799, #8280, #2872, .T. ) ;
#14703 = ORIENTED_EDGE ( 'NONE', *, *, #23772, .F. ) ;
#14704 = CARTESIAN_POINT ( 'NONE',  ( -0.7500000000000001110, 0.000000000000000000, 18.19999999999999929 ) ) ;
#14705 = CARTESIAN_POINT ( 'NONE',  ( 3.756430356250002323, 28.70312499938548356, 11.16877607737301226 ) ) ;
#14706 = CARTESIAN_POINT ( 'NONE',  ( 4.000000000000003553, 27.23124999877096641, 6.690598923241489970 ) ) ;
#14707 = AXIS2_PLACEMENT_3D ( 'NONE', #15762, #4248, #17596 ) ;
#14708 = DIRECTION ( 'NONE',  ( -0.000000000000000000, -1.000000000000000000, -0.000000000000000000 ) ) ;
#14709 = CARTESIAN_POINT ( 'NONE',  ( -3.999999999999996447, 26.57500000000000639, 8.999999999999992895 ) ) ;
#14710 = CARTESIAN_POINT ( 'NONE',  ( 15.70427213685309020, 21.01666689277176658, 11.16877607737301226 ) ) ;
#14711 = CARTESIAN_POINT ( 'NONE',  ( -3.756430356249997882, 29.00312499938548072, 11.16877607737301226 ) ) ;
#14712 = VECTOR ( 'NONE', #8889, 1000.000000000000000 ) ;
#14713 = AXIS2_PLACEMENT_3D ( 'NONE', #20784, #12940, #10975 ) ;
#14714 = DIRECTION ( 'NONE',  ( 0.000000000000000000, 0.000000000000000000, 1.000000000000000000 ) ) ;
#14715 = CYLINDRICAL_SURFACE ( 'NONE', #25791, 4.000000000000000000 ) ;
#14716 = CARTESIAN_POINT ( 'NONE',  ( 23.68807716974937705, 18.03122292025692275, 8.999999999999992895 ) ) ;
#14717 = VECTOR ( 'NONE', #863, 1000.000000000000000 ) ;
#14718 = CARTESIAN_POINT ( 'NONE',  ( 4.000000000000003553, 26.29374999877097352, 8.999999999999992895 ) ) ;
#14719 = CARTESIAN_POINT ( 'NONE',  ( 0.000000000000000000, 0.000000000000000000, 1.000000000000000000 ) ) ;
#14720 = AXIS2_PLACEMENT_3D ( 'NONE', #11873, #21943, #8088 ) ;
#14721 = CARTESIAN_POINT ( 'NONE',  ( -3.756430356250003211, -27.87812499938548427, 6.831223922626973533 ) ) ;
#14722 = DIRECTION ( 'NONE',  ( -1.000000000000000000, 0.000000000000000000, 0.000000000000000000 ) ) ;
#14723 = VERTEX_POINT ( 'NONE', #9751 ) ;
#14724 = CARTESIAN_POINT ( 'NONE',  ( 1.878215178125004048, 25.32812499938548356, 5.746835883940462963 ) ) ;
#14725 = DIRECTION ( 'NONE',  ( -0.000000000000000000, -0.000000000000000000, 1.000000000000000000 ) ) ;
#14727 = ORIENTED_EDGE ( 'NONE', *, *, #2689, .T. ) ;
#14726 = CARTESIAN_POINT ( 'NONE',  ( -1.878215178124998497, -12.25316411605951927, 0.4406249993854846614 ) ) ;
#14728 = ORIENTED_EDGE ( 'NONE', *, *, #1001, .T. ) ;
#14729 = LINE ( 'NONE', #22430, #8303 ) ;
#14730 = VECTOR ( 'NONE', #15694, 1000.000000000000000 ) ;
#14731 = CARTESIAN_POINT ( 'NONE',  ( -4.000000000000012434, -11.30940107675848516, 4.256249998770963217 ) ) ;
#14732 = ORIENTED_EDGE ( 'NONE', *, *, #20906, .T. ) ;
#14733 = CARTESIAN_POINT ( 'NONE',  ( -3.756430356250002323, -25.66562499938548569, 11.16877607737301403 ) ) ;
#14734 = CARTESIAN_POINT ( 'NONE',  ( 0.4995657836784154204, 34.50000000000000000, 3.020833333333324600 ) ) ;
#14735 = CARTESIAN_POINT ( 'NONE',  ( -1.878215178124998275, 25.44062499938549138, 12.25316411605951927 ) ) ;
#14736 = CIRCLE ( 'NONE', #10128, 26.00000000000000711 ) ;
#14737 = DIRECTION ( 'NONE',  ( 0.000000000000000000, 0.000000000000000000, -1.000000000000000000 ) ) ;
#14738 = CARTESIAN_POINT ( 'NONE',  ( 1.878215178125001605, 25.96562499938548996, 12.25316411605952283 ) ) ;
#14739 = CARTESIAN_POINT ( 'NONE',  ( 21.32489136114433848, 19.80914183329221956, 4.999999999999988454 ) ) ;
#14740 = DIRECTION ( 'NONE',  ( 0.000000000000000000, 0.000000000000000000, 1.000000000000000000 ) ) ;
#14741 = DIRECTION ( 'NONE',  ( 0.000000000000000000, -1.000000000000000000, 0.000000000000000000 ) ) ;
#14742 = AXIS2_PLACEMENT_3D ( 'NONE', #8194, #13688, #2049 ) ;
#14743 = DIRECTION ( 'NONE',  ( 0.000000000000000000, 0.000000000000000000, 1.000000000000000000 ) ) ;
#14744 = CARTESIAN_POINT ( 'NONE',  ( 4.000000000000001776, 29.89374999877097139, 8.999999999999992895 ) ) ;
#14746 = EDGE_CURVE ( 'NONE', #4195, #2907, #13135, .T. ) ;
#14745 = CARTESIAN_POINT ( 'NONE',  ( 19.12944813935283150, 19.12944813935275334, 4.662447845253954171 ) ) ;
#14747 = CARTESIAN_POINT ( 'NONE',  ( 20.83105136271035462, 15.51865660679153969, 8.999999999999992895 ) ) ;
#14748 = CARTESIAN_POINT ( 'NONE',  ( 0.000000000000000000, 0.000000000000000000, 19.50000000000000000 ) ) ;
#14749 = CARTESIAN_POINT ( 'NONE',  ( 20.46970022635141362, 14.98507572364578699, 8.999999999999992895 ) ) ;
#14750 = CARTESIAN_POINT ( 'NONE',  ( -3.756430356249996994, 27.61562499938548143, 8.999999999999992895 ) ) ;
#14751 = AXIS2_PLACEMENT_3D ( 'NONE', #21441, #17770, #25739 ) ;
#14752 = DIRECTION ( 'NONE',  ( 0.000000000000000000, 0.000000000000000000, 1.000000000000000000 ) ) ;
#14753 = CARTESIAN_POINT ( 'NONE',  ( 21.04318339706631846, 15.73078864114750530, 11.16877607737301403 ) ) ;
#14754 = CARTESIAN_POINT ( 'NONE',  ( -27.10000000000000497, 0.6000000000000000888, 19.59999999999999787 ) ) ;
#14755 = ORIENTED_EDGE ( 'NONE', *, *, #11478, .F. ) ;
#14756 = DIRECTION ( 'NONE',  ( 0.000000000000000000, 0.000000000000000000, 1.000000000000000000 ) ) ;
#14757 = CARTESIAN_POINT ( 'NONE',  ( 4.000000000000001776, 28.95624999877097494, 11.30940107675849760 ) ) ;
#14758 = CARTESIAN_POINT ( 'NONE',  ( -3.756430356250003655, -26.04062499938548569, 8.999999999999992895 ) ) ;
#14760 = ORIENTED_EDGE ( 'NONE', *, *, #19392, .T. ) ;
#14759 = CARTESIAN_POINT ( 'NONE',  ( 18.28012134629595309, 25.16042852506084770, -6.500000000000000000 ) ) ;
#14761 = DIRECTION ( 'NONE',  ( -1.000000000000000000, 0.000000000000000000, -0.000000000000000000 ) ) ;
#14762 = ADVANCED_FACE ( 'NONE', ( #9014 ), #10972, .F. ) ;
#14763 = AXIS2_PLACEMENT_3D ( 'NONE', #3563, #23308, #21359 ) ;
#14764 = EDGE_LOOP ( 'NONE', ( #10626, #11551, #7322, #20233 ) ) ;
#14765 = CARTESIAN_POINT ( 'NONE',  ( -3.735045420075836212E-15, -25.25312499938548783, 4.662447845253954171 ) ) ;
#14766 = VERTEX_POINT ( 'NONE', #12809 ) ;
#14767 = ORIENTED_EDGE ( 'NONE', *, *, #5790, .T. ) ;
#14768 = EDGE_CURVE ( 'NONE', #21315, #12001, #13836, .T. ) ;
#14769 = SURFACE_STYLE_USAGE ( .BOTH. , #8737 ) ;
#14770 = CARTESIAN_POINT ( 'NONE',  ( 3.756430356250001434, 27.50312499938548783, 8.999999999999992895 ) ) ;
#14771 = DIRECTION ( 'NONE',  ( 1.000000000000000000, 0.000000000000000000, 0.000000000000000000 ) ) ;
#14772 = EDGE_CURVE ( 'NONE', #21476, #16682, #8773, .T. ) ;
#14773 = CARTESIAN_POINT ( 'NONE',  ( 2.672651547586948120E-15, -13.33755215474602984, 2.840624999385484184 ) ) ;
#14774 =( LENGTH_UNIT ( ) NAMED_UNIT ( * ) SI_UNIT ( .MILLI., .METRE. ) );
#14775 = CARTESIAN_POINT ( 'NONE',  ( -26.00000000000000355, 0.000000000000000000, 20.00001200000000168 ) ) ;
#14776 = CARTESIAN_POINT ( 'NONE',  ( -3.756430356249996994, 28.06562499938548427, 8.999999999999992895 ) ) ;
#14777 = EDGE_CURVE ( 'NONE', #23711, #5606, #24644, .T. ) ;
#14778 = LINE ( 'NONE', #18953, #25093 ) ;
#14779 = DIRECTION ( 'NONE',  ( 0.000000000000000000, -1.000000000000000000, 0.000000000000000000 ) ) ;
#14780 = DIRECTION ( 'NONE',  ( -0.7071067811865487940, -0.7071067811865463515, 0.000000000000000000 ) ) ;
#14781 = CARTESIAN_POINT ( 'NONE',  ( 18.23893553636149534, 21.06736266110760880, 5.535898384862237620 ) ) ;
#14782 = DIRECTION ( 'NONE',  ( 0.000000000000000000, 0.000000000000000000, 1.000000000000000000 ) ) ;
#14783 = CARTESIAN_POINT ( 'NONE',  ( 1.057460391440397258E-14, -29.10624999877096641, 4.999999999999992006 ) ) ;
#14784 = CARTESIAN_POINT ( 'NONE',  ( -3.756430356250004099, -26.64062499938549067, 6.831223922626973533 ) ) ;
#14785 = DIRECTION ( 'NONE',  ( 0.9297764858882561212, 0.3681245526846659843, 0.000000000000000000 ) ) ;
#14786 = CARTESIAN_POINT ( 'NONE',  ( -14.98253926456356666, -27.25313774936403988, 1.000000000000000000 ) ) ;
#14787 = AXIS2_PLACEMENT_3D ( 'NONE', #8586, #24279, #22836 ) ;
#14788 = DIRECTION ( 'NONE',  ( 0.000000000000000000, 0.000000000000000000, 1.000000000000000000 ) ) ;
#14789 = CARTESIAN_POINT ( 'NONE',  ( -30.91344420362543843, 3.401318489841417048, 1.000000000000000000 ) ) ;
#14790 = ORIENTED_EDGE ( 'NONE', *, *, #14614, .F. ) ;
#14791 = DIRECTION ( 'NONE',  ( 0.000000000000000000, 0.000000000000000000, -1.000000000000000000 ) ) ;
#14793 = EDGE_LOOP ( 'NONE', ( #1476, #16621, #7584, #13058 ) ) ;
#14792 = FACE_OUTER_BOUND ( 'NONE', #6901, .T. ) ;
#14794 = ORIENTED_EDGE ( 'NONE', *, *, #5886, .T. ) ;
#14795 = VERTEX_POINT ( 'NONE', #21814 ) ;
#14796 = VERTEX_POINT ( 'NONE', #11601 ) ;
#14797 = ORIENTED_EDGE ( 'NONE', *, *, #11052, .T. ) ;
#14798 = DIRECTION ( 'NONE',  ( 0.000000000000000000, 0.000000000000000000, 1.000000000000000000 ) ) ;
#14799 = AXIS2_PLACEMENT_3D ( 'NONE', #4521, #24528, #20745 ) ;
#14800 = VERTEX_POINT ( 'NONE', #23518 ) ;
#14801 = EDGE_CURVE ( 'NONE', #16708, #24402, #5794, .T. ) ;
#14802 = CARTESIAN_POINT ( 'NONE',  ( -2.999999999999996891, -8.999999999999992895, 18.00000000000000000 ) ) ;
#14803 = CARTESIAN_POINT ( 'NONE',  ( 3.735045420075836212E-15, 28.96562499938548640, 4.662447845253954171 ) ) ;
#14804 = EDGE_CURVE ( 'NONE', #10376, #8478, #8299, .T. ) ;
#14805 = CARTESIAN_POINT ( 'NONE',  ( 1.878215178125004048, -5.746835883940462963, 0.6656249993854841396 ) ) ;
#14806 = CARTESIAN_POINT ( 'NONE',  ( 3.752267015613588906E-15, -4.381197846482986158, 0.5062499987709696558 ) ) ;
#14807 = CARTESIAN_POINT ( 'NONE',  ( 20.87953742278953229, 20.87953742278945768, 13.33755215474602984 ) ) ;
#14808 = EDGE_CURVE ( 'NONE', #5938, #23065, #14816, .T. ) ;
#14809 = CARTESIAN_POINT ( 'NONE',  ( -3.756430356249995661, 26.34062499938548285, 6.831223922626973533 ) ) ;
#14810 = CARTESIAN_POINT ( 'NONE',  ( 20.30280345481879323, 20.30280345481869730, 4.999999999999992006 ) ) ;
#14811 = CARTESIAN_POINT ( 'NONE',  ( 3.735045420075836212E-15, -4.662447845253954171, 3.853124999385482585 ) ) ;
#14812 = LINE ( 'NONE', #13110, #17959 ) ;
#14813 = CARTESIAN_POINT ( 'NONE',  ( 4.000000000000003553, -8.999999999999992895, 3.149999999999999911 ) ) ;
#14814 = DIRECTION ( 'NONE',  ( 0.9921147013144794302, 0.1253332335642911299, 0.000000000000000000 ) ) ;
#14815 = CARTESIAN_POINT ( 'NONE',  ( 30.10000000000000142, 0.000000000000000000, -6.500000000000000000 ) ) ;
#14816 =( BOUNDED_CURVE ( )  B_SPLINE_CURVE ( 2, ( #13463, #3897, #21430, #25730, #15411, #3511, #19196, #11482, #17637 ),
 .UNSPECIFIED., .F., .F. ) 
 B_SPLINE_CURVE_WITH_KNOTS ( ( 3, 2, 2, 2, 3 ),
 ( 0.7750000000000000222, 0.7833333333333333259, 0.8000000000000000444, 0.8166666666666666519, 0.8250000000000000666 ),
 .UNSPECIFIED. ) 
 CURVE ( )  GEOMETRIC_REPRESENTATION_ITEM ( )  RATIONAL_B_SPLINE_CURVE ( ( 0.9330127018922194093, 0.9330127018922194093, 1.000000000000000000, 0.8660254037844387076, 1.000000000000000000, 0.8660254037844387076, 1.000000000000000000, 0.9330127018922189652, 0.9330127018922194093 ) ) 
 REPRESENTATION_ITEM ( '' )  );
#14817 = CARTESIAN_POINT ( 'NONE',  ( 3.756430356250003655, -8.999999999999992895, 2.053124999385484095 ) ) ;
#14818 = CARTESIAN_POINT ( 'NONE',  ( 1.071796769724490117, -26.48259618943233562, 4.999999999999992895 ) ) ;
#14819 = ADVANCED_FACE ( 'NONE', ( #1293 ), #19456, .T. ) ;
#14820 = CARTESIAN_POINT ( 'NONE',  ( 0.000000000000000000, 0.000000000000000000, 1.000000000000000000 ) ) ;
#14821 = VERTEX_POINT ( 'NONE', #1547 ) ;
#14822 = VERTEX_POINT ( 'NONE', #23763 ) ;
#14823 = CARTESIAN_POINT ( 'NONE',  ( 2.003086131649545506E-15, 27.39062499938549067, 13.33755215474602984 ) ) ;
#14824 = EDGE_LOOP ( 'NONE', ( #11994, #10649, #18843, #12950 ) ) ;
#14825 = DIRECTION ( 'NONE',  ( 1.000000000000000000, 0.000000000000000000, -0.000000000000000000 ) ) ;
#14826 = ORIENTED_EDGE ( 'NONE', *, *, #13263, .T. ) ;
#14827 = DIRECTION ( 'NONE',  ( 0.6845471059286972748, 0.7289686274214034478, 0.000000000000000000 ) ) ;
#14828 = ORIENTED_EDGE ( 'NONE', *, *, #1500, .T. ) ;
#14829 = DIRECTION ( 'NONE',  ( -0.000000000000000000, -1.000000000000000000, -0.000000000000000000 ) ) ;
#14830 = EDGE_CURVE ( 'NONE', #7795, #4035, #9655, .T. ) ;
#14831 = ORIENTED_EDGE ( 'NONE', *, *, #14650, .F. ) ;
#14832 = CARTESIAN_POINT ( 'NONE',  ( -29.57785765677936851, -9.610428525060582317, 1.000000000000000000 ) ) ;
#14833 = CARTESIAN_POINT ( 'NONE',  ( -1.999999999999995781, 26.05000000000000071, 5.535898384862237620 ) ) ;
#14834 = CARTESIAN_POINT ( 'NONE',  ( 1.999999999999998224, -27.55000000000000071, 12.46410161513774639 ) ) ;
#14835 = EDGE_CURVE ( 'NONE', #8766, #15596, #9509, .T. ) ;
#14836 = CARTESIAN_POINT ( 'NONE',  ( -1.999999999999998224, 26.64999999999999858, 12.46410161513774639 ) ) ;
#14837 = CYLINDRICAL_SURFACE ( 'NONE', #828, 0.5000000000000001110 ) ;
#14838 = CARTESIAN_POINT ( 'NONE',  ( 21.78564551731219723, 16.47325076139337696, 8.999999999999992895 ) ) ;
#14839 = DIRECTION ( 'NONE',  ( 0.000000000000000000, 0.000000000000000000, 1.000000000000000000 ) ) ;
#14840 = CARTESIAN_POINT ( 'NONE',  ( -1.878215178124998497, 28.14062499938548356, 12.25316411605951927 ) ) ;
#14841 = ADVANCED_FACE ( 'NONE', ( #13699 ), #25230, .T. ) ;
#14842 = CARTESIAN_POINT ( 'NONE',  ( 0.000000000000000000, 0.000000000000000000, 19.00000000000000000 ) ) ;
#14843 = CYLINDRICAL_SURFACE ( 'NONE', #9978, 0.5000000000000004441 ) ;
#14844 = ORIENTED_EDGE ( 'NONE', *, *, #4355, .F. ) ;
#14845 = CARTESIAN_POINT ( 'NONE',  ( -1.999999999999995781, -5.535898384862237620, 3.243749998770965703 ) ) ;
#14846 = CARTESIAN_POINT ( 'NONE',  ( 4.000000000000005329, 25.88124999877096855, 6.690598923241489970 ) ) ;
#14847 = CARTESIAN_POINT ( 'NONE',  ( 3.756430356249997438, -26.75312499938548427, 11.16877607737301048 ) ) ;
#14848 = CARTESIAN_POINT ( 'NONE',  ( -3.137519842735244810E-15, 26.91249999999999787, 4.999999999999991118 ) ) ;
#14849 = AXIS2_PLACEMENT_3D ( 'NONE', #20548, #4590, #22648 ) ;
#14850 = CARTESIAN_POINT ( 'NONE',  ( -3.756430356249997882, 25.51562499938548356, 11.16877607737301226 ) ) ;
#14851 = CARTESIAN_POINT ( 'NONE',  ( 3.469446951953614189E-15, 39.50000000000000000, 3.999999999999991562 ) ) ;
#14853 = VERTEX_POINT ( 'NONE', #13321 ) ;
#14852 = CARTESIAN_POINT ( 'NONE',  ( 3.756430356250003655, -8.999999999999992895, 0.1406249993854830072 ) ) ;
#14854 = EDGE_LOOP ( 'NONE', ( #20245, #6848, #5144, #21214 ) ) ;
#14855 = DIRECTION ( 'NONE',  ( 0.000000000000000000, 0.000000000000000000, -1.000000000000000000 ) ) ;
#14856 = LINE ( 'NONE', #20606, #12148 ) ;
#14857 = ORIENTED_EDGE ( 'NONE', *, *, #16431, .T. ) ;
#14858 = CARTESIAN_POINT ( 'NONE',  ( 3.756430356249996105, -29.49062499938548498, 6.831223922626973533 ) ) ;
#14859 = CARTESIAN_POINT ( 'NONE',  ( 4.000000000000003553, 25.90000000000000213, 8.999999999999992895 ) ) ;
#14860 = DIRECTION ( 'NONE',  ( 0.000000000000000000, 0.000000000000000000, 1.000000000000000000 ) ) ;
#14861 = CIRCLE ( 'NONE', #13608, 27.10000000000000142 ) ;
#14862 = CARTESIAN_POINT ( 'NONE',  ( -17.87326343783916727, 25.45105997952937926, 1.000000000000000000 ) ) ;
#14863 = CARTESIAN_POINT ( 'NONE',  ( 8.012344526598182026E-15, 28.85312499938549280, 4.662447845253954171 ) ) ;
#14864 = CARTESIAN_POINT ( 'NONE',  ( 2.672651547586948120E-15, -13.33755215474602984, 4.528124999385480187 ) ) ;
#14865 = EDGE_CURVE ( 'NONE', #8603, #16823, #21297, .T. ) ;
#14866 = CARTESIAN_POINT ( 'NONE',  ( 0.000000000000000000, 0.000000000000000000, 0.000000000000000000 ) ) ;
#14867 = CARTESIAN_POINT ( 'NONE',  ( 18.06657825931632999, 20.89500538406245056, 12.46410161513774639 ) ) ;
#14868 = FACE_OUTER_BOUND ( 'NONE', #25071, .T. ) ;
#14869 = CARTESIAN_POINT ( 'NONE',  ( 0.000000000000000000, 0.000000000000000000, 1.000000000000000000 ) ) ;
#14870 = CYLINDRICAL_SURFACE ( 'NONE', #20404, 0.4999999999999970024 ) ;
#14871 = CARTESIAN_POINT ( 'NONE',  ( 17.50739442887878639, 22.81978918479745744, 8.999999999999992895 ) ) ;
#14872 = CARTESIAN_POINT ( 'NONE',  ( 16.28763523133199342, 21.60002998725066448, 6.831223922626973533 ) ) ;
#14873 = PLANE ( 'NONE',  #17226 ) ;
#14874 = FACE_OUTER_BOUND ( 'NONE', #2113, .T. ) ;
#14875 = CARTESIAN_POINT ( 'NONE',  ( -3.756430356249997882, 28.10312499938548569, 11.16877607737301226 ) ) ;
#14876 = LINE ( 'NONE', #16851, #1211 ) ;
#14877 = CARTESIAN_POINT ( 'NONE',  ( 16.66113976570983368, 19.31733714366914256, 12.25316411605951927 ) ) ;
#14878 = DIRECTION ( 'NONE',  ( 0.000000000000000000, 0.000000000000000000, 1.000000000000000000 ) ) ;
#14879 = ORIENTED_EDGE ( 'NONE', *, *, #6019, .F. ) ;
#14880 = DIRECTION ( 'NONE',  ( 0.000000000000000000, 1.000000000000000000, 0.000000000000000000 ) ) ;
#14881 = CARTESIAN_POINT ( 'NONE',  ( -3.999999999999996003, 28.73124999877096641, 6.690598923241487306 ) ) ;
#14882 = CARTESIAN_POINT ( 'NONE',  ( 3.999999999999996003, -25.18750000000000000, 6.690598923241487306 ) ) ;
#14884 = VERTEX_POINT ( 'NONE', #16062 ) ;
#14883 = DIRECTION ( 'NONE',  ( 0.000000000000000000, -0.000000000000000000, 1.000000000000000000 ) ) ;
#14885 = DIRECTION ( 'NONE',  ( 1.000000000000000000, 0.000000000000000000, 0.000000000000000000 ) ) ;
#14886 = ORIENTED_EDGE ( 'NONE', *, *, #21031, .F. ) ;
#14887 = CARTESIAN_POINT ( 'NONE',  ( 3.756430356249997882, -29.00312499938548072, 11.16877607737301226 ) ) ;
#14888 = EDGE_LOOP ( 'NONE', ( #13626, #24071, #25665, #24201 ) ) ;
#14889 = ORIENTED_EDGE ( 'NONE', *, *, #15570, .F. ) ;
#14890 = CARTESIAN_POINT ( 'NONE',  ( 0.000000000000000000, 0.000000000000000000, -6.500000000000000000 ) ) ;
#14891 = CARTESIAN_POINT ( 'NONE',  ( 1.878215178125005158, 28.47812499938549280, 5.746835883940462963 ) ) ;
#14892 = CARTESIAN_POINT ( 'NONE',  ( -8.000000000000000000, 10.00000000000000178, 15.00000000000000178 ) ) ;
#14893 = EDGE_CURVE ( 'NONE', #8412, #2690, #13270, .T. ) ;
#14894 = CARTESIAN_POINT ( 'NONE',  ( 3.756430356250003655, -8.999999999999992895, 1.603124999385485028 ) ) ;
#14895 = SHAPE_REPRESENTATION_RELATIONSHIP ( 'NONE' , 'NONE' ,  #1120, #3796 ) ;
#14896 = CARTESIAN_POINT ( 'NONE',  ( -2.000000000000000888, -27.11874999877096926, 12.46410161513774817 ) ) ;
#14897 = CARTESIAN_POINT ( 'NONE',  ( -3.756430356249997882, 28.55312499938548498, 11.16877607737301226 ) ) ;
#14898 = ADVANCED_FACE ( 'NONE', ( #18027 ), #14843, .F. ) ;
#14899 = CARTESIAN_POINT ( 'NONE',  ( -4.000000000000010658, -6.690598923241495299, 1.931249998770966814 ) ) ;
#14900 = CARTESIAN_POINT ( 'NONE',  ( 4.000000000000003553, -8.999999999999992895, 3.599999999999999201 ) ) ;
#14901 = UNCERTAINTY_MEASURE_WITH_UNIT (LENGTH_MEASURE( 1.000000000000000082E-05 ), #12798, 'distance_accuracy_value', 'NONE');
#14902 = PRODUCT_DEFINITION_CONTEXT ( 'detailed design', #21973, 'design' ) ;
#14903 = CARTESIAN_POINT ( 'NONE',  ( -1.878215178124995832, 27.99062499938548143, 5.746835883940462963 ) ) ;
#14904 = CARTESIAN_POINT ( 'NONE',  ( 29.57785765677924061, -9.610428525060996208, -6.500000000000000000 ) ) ;
#14905 = LINE ( 'NONE', #13323, #22499 ) ;
#14906 = DIRECTION ( 'NONE',  ( 0.000000000000000000, 0.000000000000000000, 1.000000000000000000 ) ) ;
#14907 = EDGE_CURVE ( 'NONE', #18639, #18972, #10763, .T. ) ;
#14908 = CARTESIAN_POINT ( 'NONE',  ( 18.03564233677035489, 18.03564233677029094, 4.999999999999992006 ) ) ;
#14909 = CARTESIAN_POINT ( 'NONE',  ( 1.878215178124998497, -27.35312499938548569, 12.25316411605951927 ) ) ;
#14910 = CARTESIAN_POINT ( 'NONE',  ( 19.94483064597403654, 19.94483064597395838, 4.999999999999992006 ) ) ;
#14911 = CARTESIAN_POINT ( 'NONE',  ( -28.34936733434187062, 12.78762572734087044, -2.750000000000000000 ) ) ;
#14912 = CARTESIAN_POINT ( 'NONE',  ( -29.99470236596024364, 8.217531866531397000, 1.000000000000000000 ) ) ;
#14913 = CARTESIAN_POINT ( 'NONE',  ( -19.32388608118446527, -23.96296185032687376, -6.500000000000000000 ) ) ;
#14914 = VERTEX_POINT ( 'NONE', #8330 ) ;
#14915 = ADVANCED_FACE ( 'NONE', ( #13969 ), #14715, .T. ) ;
#14916 = DIRECTION ( 'NONE',  ( 0.7289686274214236539, 0.6845471059286760696, 0.000000000000000000 ) ) ;
#14918 = VERTEX_POINT ( 'NONE', #8822 ) ;
#14917 = CARTESIAN_POINT ( 'NONE',  ( 14.98253926456319007, -27.25313774936425304, 1.000000000000000000 ) ) ;
#14919 = ORIENTED_EDGE ( 'NONE', *, *, #14964, .T. ) ;
#14920 = EDGE_LOOP ( 'NONE', ( #552, #20720, #11135, #10202 ) ) ;
#14921 = EDGE_LOOP ( 'NONE', ( #11762, #7099, #17900, #22435 ) ) ;
#14922 = EDGE_LOOP ( 'NONE', ( #7638, #14797 ) ) ;
#14923 = DIRECTION ( 'NONE',  ( -0.000000000000000000, -1.000000000000000000, -0.000000000000000000 ) ) ;
#14924 = ORIENTED_EDGE ( 'NONE', *, *, #21869, .T. ) ;
#14925 = CARTESIAN_POINT ( 'NONE',  ( 0.000000000000000000, 0.000000000000000000, 19.00000000000000000 ) ) ;
#14926 = FACE_OUTER_BOUND ( 'NONE', #7443, .T. ) ;
#14927 = CARTESIAN_POINT ( 'NONE',  ( 3.756430356250004099, -6.831223922626973533, 0.1781249993854828739 ) ) ;
#14928 = CARTESIAN_POINT ( 'NONE',  ( 17.79907597611823533, 23.11147073203690283, 6.831223922626973533 ) ) ;
#14929 = CARTESIAN_POINT ( 'NONE',  ( -1.878215178124995832, 25.85312499938548569, 5.746835883940462963 ) ) ;
#14930 = EDGE_CURVE ( 'NONE', #939, #8636, #4265, .T. ) ;
#14931 = CARTESIAN_POINT ( 'NONE',  ( -3.999999999999996447, -8.999999999999992895, 0.6749999999999984901 ) ) ;
#14932 = CARTESIAN_POINT ( 'NONE',  ( -1.999999999999995781, -5.535898384862237620, 0.1500000000000008271 ) ) ;
#14933 = PRODUCT_RELATED_PRODUCT_CATEGORY ( 'part', '', ( #12142 ) ) ;
#14934 = CARTESIAN_POINT ( 'NONE',  ( -16.66421332384646448, 26.25859848311288403, -6.500000000000000000 ) ) ;
#14935 = CARTESIAN_POINT ( 'NONE',  ( 3.752267015613588906E-15, -4.381197846482986158, 3.712500000000000355 ) ) ;
#14936 = CARTESIAN_POINT ( 'NONE',  ( 19.65004280752532395, 21.16579233537729721, 12.99999999999999289 ) ) ;
#14937 = CARTESIAN_POINT ( 'NONE',  ( -3.756430356249997438, -11.16877607737301048, 3.215624999385481964 ) ) ;
#14938 = CARTESIAN_POINT ( 'NONE',  ( -7.248980000273768098, 30.24338421796792176, -6.500000000000000000 ) ) ;
#14939 = CARTESIAN_POINT ( 'NONE',  ( -4.000000000000001776, -25.41250000000000142, 11.30940107675849760 ) ) ;
#14940 = ORIENTED_EDGE ( 'NONE', *, *, #9124, .T. ) ;
#14941 = ADVANCED_FACE ( 'NONE', ( #12748 ), #18158, .F. ) ;
#14942 = VERTEX_POINT ( 'NONE', #20718 ) ;
#14943 = EDGE_CURVE ( 'NONE', #19496, #16533, #24146, .T. ) ;
#14944 = ORIENTED_EDGE ( 'NONE', *, *, #389, .F. ) ;
#14945 = FACE_OUTER_BOUND ( 'NONE', #9730, .T. ) ;
#14946 = ORIENTED_EDGE ( 'NONE', *, *, #2288, .F. ) ;
#14947 = CARTESIAN_POINT ( 'NONE',  ( -21.28941499438192864, 22.67092431280617859, -6.500000000000000000 ) ) ;
#14948 = VERTEX_POINT ( 'NONE', #10160 ) ;
#14949 = DIRECTION ( 'NONE',  ( 1.000000000000000000, 0.000000000000000000, 0.000000000000000000 ) ) ;
#14950 = ORIENTED_EDGE ( 'NONE', *, *, #23227, .T. ) ;
#14951 = DIRECTION ( 'NONE',  ( 1.000000000000000000, 0.000000000000000000, 0.000000000000000000 ) ) ;
#14952 =( BOUNDED_CURVE ( )  B_SPLINE_CURVE ( 2, ( #14908, #23015, #2517, #18829, #5099, #2269, #22133, #24847, #440 ),
 .UNSPECIFIED., .F., .F. ) 
 B_SPLINE_CURVE_WITH_KNOTS ( ( 3, 2, 2, 2, 3 ),
 ( 0.02500000000000001180, 0.03333333333333333287, 0.05000000000000000278, 0.06666666666666666574, 0.07500000000000002498 ),
 .UNSPECIFIED. ) 
 CURVE ( )  GEOMETRIC_REPRESENTATION_ITEM ( )  RATIONAL_B_SPLINE_CURVE ( ( 0.9330127018922192983, 0.9330127018922194093, 1.000000000000000000, 0.8660254037844387076, 1.000000000000000000, 0.8660254037844387076, 1.000000000000000000, 0.9330127018922191873, 0.9330127018922192983 ) ) 
 REPRESENTATION_ITEM ( '' )  );
#14953 = CARTESIAN_POINT ( 'NONE',  ( 3.756430356250003655, 29.64062499938548356, 8.999999999999992895 ) ) ;
#14954 = CARTESIAN_POINT ( 'NONE',  ( -18.28012134629558716, 25.16042852506110705, 1.000000000000000000 ) ) ;
#14955 = CIRCLE ( 'NONE', #13693, 31.10000000000000142 ) ;
#14956 = CARTESIAN_POINT ( 'NONE',  ( -3.999999999999997335, 26.61250000000000071, 11.30940107675849404 ) ) ;
#14957 = DIRECTION ( 'NONE',  ( -1.000000000000000000, 0.000000000000000000, 0.000000000000000000 ) ) ;
#14958 = CARTESIAN_POINT ( 'NONE',  ( 20.80453485841585959, 15.49214010249704643, 11.16877607737301226 ) ) ;
#14959 =( BOUNDED_CURVE ( )  B_SPLINE_CURVE ( 2, ( #20893, #2980, #25075, #12791, #18802, #23237, #6774, #20763, #10949 ),
 .UNSPECIFIED., .F., .F. ) 
 B_SPLINE_CURVE_WITH_KNOTS ( ( 3, 2, 2, 2, 3 ),
 ( 0.02500000000000000139, 0.03333333333333333287, 0.05000000000000000278, 0.06666666666666666574, 0.07500000000000001110 ),
 .UNSPECIFIED. ) 
 CURVE ( )  GEOMETRIC_REPRESENTATION_ITEM ( )  RATIONAL_B_SPLINE_CURVE ( ( 0.9330127018922194093, 0.9330127018922194093, 1.000000000000000000, 0.8660254037844387076, 1.000000000000000000, 0.8660254037844387076, 1.000000000000000000, 0.9330127018922191873, 0.9330127018922192983 ) ) 
 REPRESENTATION_ITEM ( '' )  );
#14960 = CARTESIAN_POINT ( 'NONE',  ( -1.999999999999998224, 28.44999999999999929, 12.46410161513774639 ) ) ;
#14961 = CARTESIAN_POINT ( 'NONE',  ( -1.999999999999998224, 25.75000000000000355, 12.46410161513774639 ) ) ;
#14962 = CARTESIAN_POINT ( 'NONE',  ( 21.14697593998939595, 18.49077856202994852, 5.746835883940462963 ) ) ;
#14963 = DIRECTION ( 'NONE',  ( 0.000000000000000000, 0.000000000000000000, -1.000000000000000000 ) ) ;
#14964 = EDGE_CURVE ( 'NONE', #4477, #3258, #22512, .T. ) ;
#14965 = EDGE_LOOP ( 'NONE', ( #3172, #7679, #13397, #11258, #13126, #1057, #13184, #3218 ) ) ;
#14966 = CARTESIAN_POINT ( 'NONE',  ( -3.999999999999998224, 28.31874999877097210, 8.999999999999992895 ) ) ;
#14968 = EDGE_CURVE ( 'NONE', #25152, #25550, #1936, .T. ) ;
#14967 = CARTESIAN_POINT ( 'NONE',  ( 3.756430356249997438, -26.30312499938548854, 11.16877607737301048 ) ) ;
#14969 = AXIS2_PLACEMENT_3D ( 'NONE', #13844, #23771, #25484 ) ;
#14970 = CARTESIAN_POINT ( 'NONE',  ( 29.57785765677931167, 9.610428525060783045, -6.500000000000000000 ) ) ;
#14971 = CARTESIAN_POINT ( 'NONE',  ( 3.756430356250003655, 25.25312499938548427, 8.999999999999992895 ) ) ;
#14972 = LINE ( 'NONE', #22950, #15049 ) ;
#14974 = EDGE_LOOP ( 'NONE', ( #23182, #19736, #6971, #12175 ) ) ;
#14973 = CARTESIAN_POINT ( 'NONE',  ( 3.756430356250004099, 28.89062499938549067, 6.831223922626973533 ) ) ;
#14975 = ORIENTED_EDGE ( 'NONE', *, *, #24355, .T. ) ;
#14976 = CARTESIAN_POINT ( 'NONE',  ( 30.78811501957141772, -4.393401135981229721, -2.750000000000000000 ) ) ;
#14977 = AXIS2_PLACEMENT_3D ( 'NONE', #5386, #15466, #7739 ) ;
#14978 = DIRECTION ( 'NONE',  ( 0.000000000000000000, 0.000000000000000000, -1.000000000000000000 ) ) ;
#14979 = AXIS2_PLACEMENT_3D ( 'NONE', #9900, #5986, #17886 ) ;
#14980 = VERTEX_POINT ( 'NONE', #359 ) ;
#14981 = FACE_OUTER_BOUND ( 'NONE', #18207, .T. ) ;
#14982 = CARTESIAN_POINT ( 'NONE',  ( 2.000000000000003997, 25.97500000000000142, 5.535898384862238508 ) ) ;
#14983 = CARTESIAN_POINT ( 'NONE',  ( -2.003086131649545506E-15, 26.37812499938548427, 13.33755215474603162 ) ) ;
#14984 = LINE ( 'NONE', #17346, #8950 ) ;
#14985 = CARTESIAN_POINT ( 'NONE',  ( 0.000000000000000000, 28.62812499938549138, 13.33755215474602984 ) ) ;
#14986 = VECTOR ( 'NONE', #1129, 1000.000000000000000 ) ;
#14987 = CARTESIAN_POINT ( 'NONE',  ( 2.000000000000005329, 25.52500000000000568, 5.535898384862238508 ) ) ;
#14988 = CIRCLE ( 'NONE', #23728, 31.10000000000000142 ) ;
#14989 = DIRECTION ( 'NONE',  ( 0.000000000000000000, 0.000000000000000000, 1.000000000000000000 ) ) ;
#14990 = CARTESIAN_POINT ( 'NONE',  ( -3.999999999999996447, -8.999999999999992895, 2.418749998770966414 ) ) ;
#14991 = CIRCLE ( 'NONE', #15402, 0.4999999999999992784 ) ;
#14992 = CYLINDRICAL_SURFACE ( 'NONE', #5493, 0.5000000000000004441 ) ;
#14993 = CARTESIAN_POINT ( 'NONE',  ( 3.756430356250003211, 26.52812499938548285, 6.831223922626973533 ) ) ;
#14994 = CIRCLE ( 'NONE', #5395, 31.10000000000000142 ) ;
#14995 = LINE ( 'NONE', #8986, #17902 ) ;
#14996 = CARTESIAN_POINT ( 'NONE',  ( 23.29708626209844269, 17.98469150617961887, 8.999999999999992895 ) ) ;
#14997 = CARTESIAN_POINT ( 'NONE',  ( 16.95282131294928263, 19.60901869090858796, 5.746835883940462963 ) ) ;
#14998 = EDGE_CURVE ( 'NONE', #21622, #21212, #7627, .T. ) ;
#14999 = CARTESIAN_POINT ( 'NONE',  ( 23.68807716974937705, 18.03122292025692275, 8.999999999999992895 ) ) ;
#15000 = CARTESIAN_POINT ( 'NONE',  ( 3.756430356250004099, 28.32812499938548356, 6.831223922626973533 ) ) ;
#15001 = CARTESIAN_POINT ( 'NONE',  ( 23.72661691079926527, 18.35913567140812575, 7.710170883190207824 ) ) ;
#15002 = CARTESIAN_POINT ( 'NONE',  ( 22.63417365473605614, 17.32177889881723587, 11.16877607737301403 ) ) ;
#15003 = CARTESIAN_POINT ( 'NONE',  ( 22.18105584147648912, 19.35262871673023000, 12.46410161513774817 ) ) ;
#15004 = EDGE_LOOP ( 'NONE', ( #16982, #17310, #5000, #10110 ) ) ;
#15005 = DIRECTION ( 'NONE',  ( 0.000000000000000000, 0.000000000000000000, 1.000000000000000000 ) ) ;
#15006 = CARTESIAN_POINT ( 'NONE',  ( 4.000000000000003553, 29.03124999877096712, 6.690598923241489970 ) ) ;
#15007 = CARTESIAN_POINT ( 'NONE',  ( -3.756430356250002323, -29.60312499938548569, 11.16877607737301226 ) ) ;
#15009 = ORIENTED_EDGE ( 'NONE', *, *, #2436, .T. ) ;
#15008 = DIRECTION ( 'NONE',  ( -0.000000000000000000, 0.000000000000000000, 1.000000000000000000 ) ) ;
#15010 = CARTESIAN_POINT ( 'NONE',  ( 3.469446951953614189E-15, 39.50000000000000000, 3.999999999999991562 ) ) ;
#15011 = EDGE_CURVE ( 'NONE', #17619, #13585, #12065, .T. ) ;
#15012 = AXIS2_PLACEMENT_3D ( 'NONE', #20792, #23267, #13088 ) ;
#15013 = ORIENTED_EDGE ( 'NONE', *, *, #7648, .T. ) ;
#15014 = CARTESIAN_POINT ( 'NONE',  ( -3.756430356250004099, -28.32812499938548356, 6.831223922626973533 ) ) ;
#15015 = ORIENTED_EDGE ( 'NONE', *, *, #10791, .T. ) ;
#15016 = VERTEX_POINT ( 'NONE', #12256 ) ;
#15017 = CARTESIAN_POINT ( 'NONE',  ( 19.26088974974303625, 23.00113871462370341, 5.987824696368042154 ) ) ;
#15018 = CARTESIAN_POINT ( 'NONE',  ( 3.756430356250004987, 27.95312499938548711, 8.999999999999992895 ) ) ;
#15019 = EDGE_CURVE ( 'NONE', #16342, #23081, #15961, .T. ) ;
#15020 = VECTOR ( 'NONE', #20323, 1000.000000000000000 ) ;
#15021 = CARTESIAN_POINT ( 'NONE',  ( -1.878215178124995832, -5.746835883940462963, 1.190624999385481830 ) ) ;
#15022 = AXIS2_PLACEMENT_3D ( 'NONE', #4448, #6666, #22765 ) ;
#15023 = CARTESIAN_POINT ( 'NONE',  ( 3.756430356250003655, -8.999999999999992895, 3.403124999385484628 ) ) ;
#15024 = SURFACE_SIDE_STYLE ('',( #16871 ) ) ;
#15025 = CARTESIAN_POINT ( 'NONE',  ( 0.000000000000000000, 0.000000000000000000, -6.500000000000000000 ) ) ;
#15026 = VECTOR ( 'NONE', #3755, 1000.000000000000000 ) ;
#15027 = CARTESIAN_POINT ( 'NONE',  ( -3.756430356249997882, 29.00312499938548072, 11.16877607737301226 ) ) ;
#15028 = CARTESIAN_POINT ( 'NONE',  ( 20.53261315870440384, 14.87575890921195665, 6.690598923241489970 ) ) ;
#15029 = CIRCLE ( 'NONE', #395, 0.4999999999999997224 ) ;
#15030 = CARTESIAN_POINT ( 'NONE',  ( 3.469446951953614189E-15, 30.00000000000000355, 8.999999999999992895 ) ) ;
#15031 = CARTESIAN_POINT ( 'NONE',  ( 3.756430356250003655, 29.19062499938548072, 8.999999999999992895 ) ) ;
#15032 = CARTESIAN_POINT ( 'NONE',  ( -30.12293631110035363, 7.734255490827311341, -6.500000000000000000 ) ) ;
#15033 = DIRECTION ( 'NONE',  ( -0.000000000000000000, -0.000000000000000000, 1.000000000000000000 ) ) ;
#15034 = CARTESIAN_POINT ( 'NONE',  ( -29.57785765677936851, -9.610428525060582317, -6.500000000000000000 ) ) ;
#15035 = LINE ( 'NONE', #12447, #14298 ) ;
#15036 = CARTESIAN_POINT ( 'NONE',  ( 1.878215178124995832, -26.30312499938548498, 5.746835883940462963 ) ) ;
#15037 = CARTESIAN_POINT ( 'NONE',  ( 1.878215178125004048, 25.77812499938548640, 5.746835883940462963 ) ) ;
#15038 = CIRCLE ( 'NONE', #3749, 0.5000000000000004441 ) ;
#15039 = CARTESIAN_POINT ( 'NONE',  ( 0.000000000000000000, 0.000000000000000000, -6.500000000000000000 ) ) ;
#15041 = CARTESIAN_POINT ( 'NONE',  ( -3.999999999999997335, 26.10624999877096997, 11.30940107675849404 ) ) ;
#15040 = AXIS2_PLACEMENT_3D ( 'NONE', #15597, #1982, #11652 ) ;
#15042 = FACE_OUTER_BOUND ( 'NONE', #22369, .T. ) ;
#15043 = ORIENTED_EDGE ( 'NONE', *, *, #13095, .F. ) ;
#15044 = CARTESIAN_POINT ( 'NONE',  ( -5.357848403820182348, 38.93885650637880502, 7.509366431266231601 ) ) ;
#15046 = VERTEX_POINT ( 'NONE', #19134 ) ;
#15045 = DIRECTION ( 'NONE',  ( -0.000000000000000000, 0.000000000000000000, -1.000000000000000000 ) ) ;
#15048 = ORIENTED_EDGE ( 'NONE', *, *, #3089, .F. ) ;
#15047 = EDGE_CURVE ( 'NONE', #25045, #284, #13256, .T. ) ;
#15049 = VECTOR ( 'NONE', #5288, 1000.000000000000000 ) ;
#15050 = ORIENTED_EDGE ( 'NONE', *, *, #3988, .F. ) ;
#15051 = VERTEX_POINT ( 'NONE', #17440 ) ;
#15052 = EDGE_LOOP ( 'NONE', ( #1663, #19661, #13182, #3814 ) ) ;
#15053 = DIRECTION ( 'NONE',  ( 0.000000000000000000, -1.000000000000000000, -0.000000000000000000 ) ) ;
#15054 = AXIS2_PLACEMENT_3D ( 'NONE', #7844, #15829, #3542 ) ;
#15055 = DIRECTION ( 'NONE',  ( -0.000000000000000000, 0.000000000000000000, 1.000000000000000000 ) ) ;
#15056 = EDGE_CURVE ( 'NONE', #11588, #19628, #15103, .T. ) ;
#15057 = AXIS2_PLACEMENT_3D ( 'NONE', #14239, #22599, #14619 ) ;
#15058 = EDGE_LOOP ( 'NONE', ( #19945, #9910, #8352, #1885, #1564 ) ) ;
#15059 = EDGE_CURVE ( 'NONE', #11742, #7537, #5027, .T. ) ;
#15060 = CARTESIAN_POINT ( 'NONE',  ( 3.735045420075836212E-15, 29.41562499938548569, 4.662447845253954171 ) ) ;
#15061 = AXIS2_PLACEMENT_3D ( 'NONE', #5186, #1251, #13162 ) ;
#15062 = CARTESIAN_POINT ( 'NONE',  ( -1.878215178124995832, -5.746835883940462963, 1.190624999385481830 ) ) ;
#15063 = CARTESIAN_POINT ( 'NONE',  ( -1.999999999999995781, -5.535898384862237620, 2.343749998770968013 ) ) ;
#15064 = CARTESIAN_POINT ( 'NONE',  ( 22.66069015903055117, 17.34829540311172735, 8.999999999999992895 ) ) ;
#15065 = EDGE_CURVE ( 'NONE', #16682, #16342, #3067, .T. ) ;
#15066 = CARTESIAN_POINT ( 'NONE',  ( 3.756430356250004099, 25.29062499938548569, 6.831223922626973533 ) ) ;
#15067 = CARTESIAN_POINT ( 'NONE',  ( -19.58805710660146104, -17.18149551509901940, 20.00001200000000168 ) ) ;
#15068 = CIRCLE ( 'NONE', #18393, 4.000000000000000000 ) ;
#15069 = CARTESIAN_POINT ( 'NONE',  ( -1.878215178124995832, -5.746835883940462963, 3.440624999385483829 ) ) ;
#15070 = DIRECTION ( 'NONE',  ( 0.000000000000000000, 0.000000000000000000, 1.000000000000000000 ) ) ;
#15071 = LINE ( 'NONE', #7342, #23314 ) ;
#15072 = CARTESIAN_POINT ( 'NONE',  ( 0.000000000000000000, 0.000000000000000000, -6.500000000000000000 ) ) ;
#15073 = LINE ( 'NONE', #14815, #23424 ) ;
#15074 = CARTESIAN_POINT ( 'NONE',  ( 3.756430356250003655, -8.999999999999992895, 3.853124999385483473 ) ) ;
#15075 = AXIS2_PLACEMENT_3D ( 'NONE', #7628, #13905, #11668 ) ;
#15076 = DIRECTION ( 'NONE',  ( 0.06279051952930848890, -0.9980267284282718920, 0.000000000000000000 ) ) ;
#15077 = ORIENTED_EDGE ( 'NONE', *, *, #10468, .T. ) ;
#15078 = EDGE_CURVE ( 'NONE', #3783, #14500, #12472, .T. ) ;
#15079 = ORIENTED_EDGE ( 'NONE', *, *, #18724, .T. ) ;
#15080 = ORIENTED_EDGE ( 'NONE', *, *, #22316, .F. ) ;
#15081 = CARTESIAN_POINT ( 'NONE',  ( -1.952785157361865753, -31.03863125411923463, -6.500000000000000000 ) ) ;
#15082 = EDGE_LOOP ( 'NONE', ( #372, #12912, #8608, #13375 ) ) ;
#15083 = CARTESIAN_POINT ( 'NONE',  ( 3.756430356249997882, -26.41562499938548569, 11.16877607737301226 ) ) ;
#15084 = ORIENTED_EDGE ( 'NONE', *, *, #11177, .T. ) ;
#15085 = DIRECTION ( 'NONE',  ( 0.000000000000000000, -1.000000000000000000, 0.000000000000000000 ) ) ;
#15086 = EDGE_CURVE ( 'NONE', #24580, #9729, #24595, .T. ) ;
#15087 = ORIENTED_EDGE ( 'NONE', *, *, #5330, .F. ) ;
#15088 = CARTESIAN_POINT ( 'NONE',  ( -1.499999999999998224, -10.49999999999999289, 4.999999999999993783 ) ) ;
#15089 = ADVANCED_FACE ( 'NONE', ( #11287 ), #24905, .T. ) ;
#15090 = CARTESIAN_POINT ( 'NONE',  ( -3.999999999999997335, 25.26249999999999929, 11.30940107675849404 ) ) ;
#15091 = CARTESIAN_POINT ( 'NONE',  ( -1.626862140677534194E-14, -27.58750000000000213, 12.99999999999999289 ) ) ;
#15092 = VECTOR ( 'NONE', #9405, 1000.000000000000000 ) ;
#15093 = AXIS2_PLACEMENT_3D ( 'NONE', #8791, #693, #3040 ) ;
#15094 = CYLINDRICAL_SURFACE ( 'NONE', #7165, 0.5000000000000004441 ) ;
#15095 = DIRECTION ( 'NONE',  ( -0.000000000000000000, -0.000000000000000000, -1.000000000000000000 ) ) ;
#15096 = CARTESIAN_POINT ( 'NONE',  ( 21.75912901301770219, 16.44673425709888548, 11.16877607737301226 ) ) ;
#15097 = ADVANCED_FACE ( 'NONE', ( #9074 ), #21371, .F. ) ;
#15099 = EDGE_CURVE ( 'NONE', #7296, #19084, #15230, .T. ) ;
#15098 = AXIS2_PLACEMENT_3D ( 'NONE', #11176, #23222, #1254 ) ;
#15100 = FACE_OUTER_BOUND ( 'NONE', #16894, .T. ) ;
#15101 = CARTESIAN_POINT ( 'NONE',  ( 2.000000000000000888, 26.27499999999999858, 12.46410161513774817 ) ) ;
#15102 = CARTESIAN_POINT ( 'NONE',  ( 18.01348148472910893, 20.66967886268841426, 12.25316411605951927 ) ) ;
#15103 = LINE ( 'NONE', #7370, #24122 ) ;
#15104 = AXIS2_PLACEMENT_3D ( 'NONE', #2673, #6333, #6714 ) ;
#15105 = ORIENTED_EDGE ( 'NONE', *, *, #14577, .F. ) ;
#15106 = VERTEX_POINT ( 'NONE', #12868 ) ;
#15107 = CARTESIAN_POINT ( 'NONE',  ( 4.000000000000002665, 28.13124999877096855, 6.690598923241489970 ) ) ;
#15108 = VECTOR ( 'NONE', #17772, 1000.000000000000000 ) ;
#15109 = CARTESIAN_POINT ( 'NONE',  ( 3.756430356249996994, -28.51562499938548356, 8.999999999999992895 ) ) ;
#15110 = AXIS2_PLACEMENT_3D ( 'NONE', #7359, #21215, #9711 ) ;
#15111 = CARTESIAN_POINT ( 'NONE',  ( -1.999999999999995781, 26.95000000000000284, 5.535898384862237620 ) ) ;
#15112 = CARTESIAN_POINT ( 'NONE',  ( 3.756430356250002323, 27.01562499938548356, 11.16877607737301226 ) ) ;
#15113 = LINE ( 'NONE', #14851, #12114 ) ;
#15115 = ORIENTED_EDGE ( 'NONE', *, *, #7428, .T. ) ;
#15114 = CARTESIAN_POINT ( 'NONE',  ( -25.98730014090454432, -17.08421000182750760, -6.500000000000000000 ) ) ;
#15116 = ORIENTED_EDGE ( 'NONE', *, *, #21632, .T. ) ;
#15117 =( BOUNDED_CURVE ( )  B_SPLINE_CURVE ( 2, ( #1163, #5480, #13474, #21440, #24969, #3520, #23527, #19465, #1556 ),
 .UNSPECIFIED., .F., .F. ) 
 B_SPLINE_CURVE_WITH_KNOTS ( ( 3, 2, 2, 2, 3 ),
 ( 0.4750000000000000333, 0.4833333333333333370, 0.5000000000000000000, 0.5166666666666667185, 0.5250000000000000222 ),
 .UNSPECIFIED. ) 
 CURVE ( )  GEOMETRIC_REPRESENTATION_ITEM ( )  RATIONAL_B_SPLINE_CURVE ( ( 0.9330127018922194093, 0.9330127018922196314, 1.000000000000000000, 0.8660254037844387076, 1.000000000000000000, 0.8660254037844387076, 1.000000000000000000, 0.9330127018922194093, 0.9330127018922194093 ) ) 
 REPRESENTATION_ITEM ( '' )  );
#15118 = DIRECTION ( 'NONE',  ( 1.000000000000000000, 0.000000000000000000, 0.000000000000000000 ) ) ;
#15119 = AXIS2_PLACEMENT_3D ( 'NONE', #11359, #3765, #1432 ) ;
#15120 = CYLINDRICAL_SURFACE ( 'NONE', #17172, 31.10000000000000142 ) ;
#15121 = VERTEX_POINT ( 'NONE', #17326 ) ;
#15122 = CARTESIAN_POINT ( 'NONE',  ( -3.756430356250002323, -28.36562499938548854, 11.16877607737301403 ) ) ;
#15123 = CARTESIAN_POINT ( 'NONE',  ( 1.878215178125006934, 29.26562499938549067, 5.746835883940462963 ) ) ;
#15124 =( BOUNDED_SURFACE ( )  B_SPLINE_SURFACE ( 1, 2, ( 
 ( #9717, #3956, #21607, #1875, #9836, #17701, #10090, #17819, #15731, #25784, #7869, #18090, #7487, #3685, #11665, #5916, #15476, #3565, #21874, #11538, #23827, #19891, #1990, #8012, #17564, #36, #15997, #7624, #19505, #25669, #23694, #9958, #23964, #4206, #24214, #428, #24352, #4740, #4461, #12713, #6301, #12436, #6681, #12185, #24082, #20403, #10472, #2258, #18473, #8532, #14671, #8396, #16119, #10214, #22652, #20552, #561, #24594, #18212, #20680, #16386, #2506, #6164, #2379, #4593, #16513, #293, #8263, #24475, #12314, #6552, #14534, #8142, #22511, #20158, #12572, #2644, #10605, #18595, #14294, #20282, #22259, #2763, #4340, #10333, #682, #16242, #18329, #10724, #14152, #6432, #8649, #14419, #16628, #171, #22120, #22377, #8780, #2889, #7332, #13221, #19097, #17288, #20806, #15312, #18980, #21075, #16769, #20946, #23162, #1181, #10858, #18854, #9161, #4985, #25122, #13101, #801, #3152, #12832, #17151 ),
 ( #12965, #14927, #21327, #6948, #16903, #7210, #945, #8923, #25253, #24738, #22779, #1065, #23280, #24867, #14805, #15192, #22899, #24986, #3031, #6823, #5362, #5242, #13351, #9038, #7071, #17021, #4856, #11000, #15062, #3405, #23037, #5125, #11118, #18710, #19223, #21191, #3268, #11243, #1323, #9303, #5882, #17404, #21966, #3536, #25369, #23931, #17529, #17911, #13609, #7837, #1572, #5744, #13725, #21574, #6013, #21706, #19607, #3791, #15701, #9924, #11383, #9543, #25503, #9807, #19358, #1453, #25755, #2, #11768, #25637, #23793, #11893, #13491, #3922, #19862, #11507, #9424, #19478, #7977, #19746, #9683, #15440, #7592, #11630, #17669, #15963, #23667, #13993, #15577, #1845, #7453, #23413, #5498, #17789, #21459, #15821, #23545, #1960, #5628, #13866, #21841, #3653, #1710, #7718, #18780, #2348, #2091, #6135, #8850, #18057, #8114, #6398, #2227, #16088, #24051, #141, #10785, #14864, #20250, #14120, #4042 ) ),
 .UNSPECIFIED., .F., .F., .F. ) 
 B_SPLINE_SURFACE_WITH_KNOTS ( ( 2, 2 ),
 ( 3, 2, 2, 2, 2, 2, 2, 2, 2, 2, 2, 2, 2, 2, 2, 2, 2, 2, 2, 2, 2, 2, 2, 2, 2, 2, 2, 2, 2, 2, 2, 2, 2, 2, 2, 2, 2, 2, 2, 2, 2, 2, 2, 2, 2, 2, 2, 2, 2, 2, 2, 2, 2, 2, 2, 2, 2, 2, 2, 2, 3 ),
 ( 0.000000000000000000, 1.000000000000000000 ),
 ( 0.000000000000000000, 0.01666666666666666644, 0.03333333333333333287, 0.05000000000000000278, 0.06666666666666666574, 0.08333333333333332871, 0.1000000000000000056, 0.1166666666666666685, 0.1333333333333333315, 0.1499999999999999944, 0.1666666666666666574, 0.1833333333333333204, 0.2000000000000000111, 0.2166666666666666741, 0.2333333333333333370, 0.2500000000000000000, 0.2666666666666666630, 0.2833333333333333259, 0.2999999999999999889, 0.3166666666666666519, 0.3333333333333333148, 0.3499999999999999778, 0.3666666666666666408, 0.3833333333333333592, 0.4000000000000000222, 0.4166666666666666852, 0.4333333333333333481, 0.4500000000000000111, 0.4666666666666666741, 0.4833333333333333370, 0.5000000000000000000, 0.5166666666666667185, 0.5333333333333333259, 0.5500000000000000444, 0.5666666666666666519, 0.5833333333333333703, 0.5999999999999999778, 0.6166666666666666963, 0.6333333333333333037, 0.6500000000000000222, 0.6666666666666666297, 0.6833333333333333481, 0.6999999999999999556, 0.7166666666666666741, 0.7333333333333332815, 0.7500000000000000000, 0.7666666666666667185, 0.7833333333333333259, 0.8000000000000000444, 0.8166666666666666519, 0.8333333333333333703, 0.8499999999999999778, 0.8666666666666666963, 0.8833333333333333037, 0.9000000000000000222, 0.9166666666666666297, 0.9333333333333333481, 0.9499999999999999556, 0.9666666666666666741, 0.9833333333333332815, 1.000000000000000000 ),
 .UNSPECIFIED. ) 
 GEOMETRIC_REPRESENTATION_ITEM ( )  RATIONAL_B_SPLINE_SURFACE ( (
 ( 1.000000000000000000, 0.8660254037844387076, 1.000000000000000000, 0.8660254037844387076, 1.000000000000000000, 0.8660254037844387076, 1.000000000000000000, 0.8660254037844387076, 1.000000000000000000, 0.8660254037844387076, 1.000000000000000000, 0.8660254037844387076, 1.000000000000000000, 0.8660254037844387076, 1.000000000000000000, 0.8660254037844387076, 1.000000000000000000, 0.8660254037844387076, 1.000000000000000000, 0.8660254037844387076, 1.000000000000000000, 0.8660254037844387076, 1.000000000000000000, 0.8660254037844387076, 1.000000000000000000, 0.8660254037844387076, 1.000000000000000000, 0.8660254037844387076, 1.000000000000000000, 0.8660254037844387076, 1.000000000000000000, 0.8660254037844387076, 1.000000000000000000, 0.8660254037844387076, 1.000000000000000000, 0.8660254037844387076, 1.000000000000000000, 0.8660254037844387076, 1.000000000000000000, 0.8660254037844387076, 1.000000000000000000, 0.8660254037844387076, 1.000000000000000000, 0.8660254037844387076, 1.000000000000000000, 0.8660254037844387076, 1.000000000000000000, 0.8660254037844387076, 1.000000000000000000, 0.8660254037844387076, 1.000000000000000000, 0.8660254037844387076, 1.000000000000000000, 0.8660254037844387076, 1.000000000000000000, 0.8660254037844387076, 1.000000000000000000, 0.8660254037844387076, 1.000000000000000000, 0.8660254037844387076, 1.000000000000000000, 0.8660254037844387076, 1.000000000000000000, 0.8660254037844387076, 1.000000000000000000, 0.8660254037844387076, 1.000000000000000000, 0.8660254037844387076, 1.000000000000000000, 0.8660254037844387076, 1.000000000000000000, 0.8660254037844387076, 1.000000000000000000, 0.8660254037844387076, 1.000000000000000000, 0.8660254037844387076, 1.000000000000000000, 0.8660254037844387076, 1.000000000000000000, 0.8660254037844387076, 1.000000000000000000, 0.8660254037844387076, 1.000000000000000000, 0.8660254037844387076, 1.000000000000000000, 0.8660254037844387076, 1.000000000000000000, 0.8660254037844387076, 1.000000000000000000, 0.8660254037844387076, 1.000000000000000000, 0.8660254037844387076, 1.000000000000000000, 0.8660254037844387076, 1.000000000000000000, 0.8660254037844387076, 1.000000000000000000, 0.8660254037844387076, 1.000000000000000000, 0.8660254037844387076, 1.000000000000000000, 0.8660254037844387076, 1.000000000000000000, 0.8660254037844387076, 1.000000000000000000, 0.8660254037844387076, 1.000000000000000000, 0.8660254037844387076, 1.000000000000000000, 0.8660254037844387076, 1.000000000000000000, 0.8660254037844387076, 1.000000000000000000, 0.8660254037844387076, 1.000000000000000000, 0.8660254037844387076, 1.000000000000000000, 0.8660254037844387076, 1.000000000000000000, 0.8660254037844387076, 1.000000000000000000),
 ( 1.000000000000000000, 0.8660254037844387076, 1.000000000000000000, 0.8660254037844387076, 1.000000000000000000, 0.8660254037844387076, 1.000000000000000000, 0.8660254037844387076, 1.000000000000000000, 0.8660254037844387076, 1.000000000000000000, 0.8660254037844387076, 1.000000000000000000, 0.8660254037844387076, 1.000000000000000000, 0.8660254037844387076, 1.000000000000000000, 0.8660254037844387076, 1.000000000000000000, 0.8660254037844387076, 1.000000000000000000, 0.8660254037844387076, 1.000000000000000000, 0.8660254037844387076, 1.000000000000000000, 0.8660254037844387076, 1.000000000000000000, 0.8660254037844387076, 1.000000000000000000, 0.8660254037844387076, 1.000000000000000000, 0.8660254037844387076, 1.000000000000000000, 0.8660254037844387076, 1.000000000000000000, 0.8660254037844387076, 1.000000000000000000, 0.8660254037844387076, 1.000000000000000000, 0.8660254037844387076, 1.000000000000000000, 0.8660254037844387076, 1.000000000000000000, 0.8660254037844387076, 1.000000000000000000, 0.8660254037844387076, 1.000000000000000000, 0.8660254037844387076, 1.000000000000000000, 0.8660254037844387076, 1.000000000000000000, 0.8660254037844387076, 1.000000000000000000, 0.8660254037844387076, 1.000000000000000000, 0.8660254037844387076, 1.000000000000000000, 0.8660254037844387076, 1.000000000000000000, 0.8660254037844387076, 1.000000000000000000, 0.8660254037844387076, 1.000000000000000000, 0.8660254037844387076, 1.000000000000000000, 0.8660254037844387076, 1.000000000000000000, 0.8660254037844387076, 1.000000000000000000, 0.8660254037844387076, 1.000000000000000000, 0.8660254037844387076, 1.000000000000000000, 0.8660254037844387076, 1.000000000000000000, 0.8660254037844387076, 1.000000000000000000, 0.8660254037844387076, 1.000000000000000000, 0.8660254037844387076, 1.000000000000000000, 0.8660254037844387076, 1.000000000000000000, 0.8660254037844387076, 1.000000000000000000, 0.8660254037844387076, 1.000000000000000000, 0.8660254037844387076, 1.000000000000000000, 0.8660254037844387076, 1.000000000000000000, 0.8660254037844387076, 1.000000000000000000, 0.8660254037844387076, 1.000000000000000000, 0.8660254037844387076, 1.000000000000000000, 0.8660254037844387076, 1.000000000000000000, 0.8660254037844387076, 1.000000000000000000, 0.8660254037844387076, 1.000000000000000000, 0.8660254037844387076, 1.000000000000000000, 0.8660254037844387076, 1.000000000000000000, 0.8660254037844387076, 1.000000000000000000, 0.8660254037844387076, 1.000000000000000000, 0.8660254037844387076, 1.000000000000000000, 0.8660254037844387076, 1.000000000000000000, 0.8660254037844387076, 1.000000000000000000, 0.8660254037844387076, 1.000000000000000000, 0.8660254037844387076, 1.000000000000000000) ) ) 
 REPRESENTATION_ITEM ( '' )  SURFACE ( )  );
#15125 = CARTESIAN_POINT ( 'NONE',  ( -1.878215178124998275, 25.89062499938549067, 12.25316411605951927 ) ) ;
#15126 = LINE ( 'NONE', #7515, #25534 ) ;
#15127 = CARTESIAN_POINT ( 'NONE',  ( 0.000000000000000000, 29.52812499938548640, 13.33755215474602984 ) ) ;
#15128 = EDGE_CURVE ( 'NONE', #4507, #3917, #8735, .T. ) ;
#15129 = CIRCLE ( 'NONE', #3007, 0.5000000000000004441 ) ;
#15130 = EDGE_CURVE ( 'NONE', #18321, #20266, #20796, .T. ) ;
#15131 = AXIS2_PLACEMENT_3D ( 'NONE', #11604, #23766, #25478 ) ;
#15132 = DIRECTION ( 'NONE',  ( -0.000000000000000000, -0.000000000000000000, 1.000000000000000000 ) ) ;
#15133 = SHAPE_DEFINITION_REPRESENTATION ( #17993, #23343 ) ;
#15134 = VECTOR ( 'NONE', #2816, 1000.000000000000000 ) ;
#15135 = CARTESIAN_POINT ( 'NONE',  ( 17.08421000182759997, -25.98730014090448392, 1.000000000000000000 ) ) ;
#15136 = EDGE_CURVE ( 'NONE', #7090, #14766, #19014, .T. ) ;
#15137 = DIRECTION ( 'NONE',  ( -1.000000000000000000, -0.000000000000000000, -0.000000000000000000 ) ) ;
#15138 = CARTESIAN_POINT ( 'NONE',  ( -3.756430356249996105, 27.12812499938548427, 6.831223922626973533 ) ) ;
#15139 = CARTESIAN_POINT ( 'NONE',  ( 3.469446951953614189E-15, 30.00000000000000355, 4.999999999999992006 ) ) ;
#15140 = CARTESIAN_POINT ( 'NONE',  ( 15.32653948221845575, 20.98339373171076971, 8.999999999999992895 ) ) ;
#15141 = CARTESIAN_POINT ( 'NONE',  ( 21.49396397007274473, 16.18156921415393157, 6.831223922626973533 ) ) ;
#15142 = DIRECTION ( 'NONE',  ( -0.7071067811865487940, -0.7071067811865463515, 0.000000000000000000 ) ) ;
#15143 = CARTESIAN_POINT ( 'NONE',  ( 1.878215178125000939, 28.21562499938548640, 12.25316411605952283 ) ) ;
#15144 = DIRECTION ( 'NONE',  ( 0.5358267949790093132, 0.8443279255020070817, 0.000000000000000000 ) ) ;
#15145 = VECTOR ( 'NONE', #7328, 1000.000000000000000 ) ;
#15146 = CARTESIAN_POINT ( 'NONE',  ( 16.89751483010538990, 22.20990958602406096, 11.16877607737301048 ) ) ;
#15147 = LINE ( 'NONE', #16853, #13389 ) ;
#15148 = ORIENTED_EDGE ( 'NONE', *, *, #8590, .T. ) ;
#15149 = CARTESIAN_POINT ( 'NONE',  ( -1.999999999999995781, 25.54374999877096997, 5.535898384862237620 ) ) ;
#15150 = CARTESIAN_POINT ( 'NONE',  ( 4.000000000000003553, 28.99374999877096926, 8.999999999999992895 ) ) ;
#15151 = CARTESIAN_POINT ( 'NONE',  ( -3.756430356250004099, -29.22812499938548925, 6.831223922626973533 ) ) ;
#15153 = ORIENTED_EDGE ( 'NONE', *, *, #5958, .T. ) ;
#15152 = CARTESIAN_POINT ( 'NONE',  ( -1.859271017917182139E-15, -29.38749999999999929, 12.99999999999999289 ) ) ;
#15154 = CARTESIAN_POINT ( 'NONE',  ( 3.834746474454188013E-15, 26.40624999877096357, 4.999999999999992006 ) ) ;
#15155 = CIRCLE ( 'NONE', #24737, 31.10000000000000142 ) ;
#15156 = VERTEX_POINT ( 'NONE', #23079 ) ;
#15157 = CARTESIAN_POINT ( 'NONE',  ( 1.878215178124995832, -29.34062499938548285, 5.746835883940462963 ) ) ;
#15158 = ORIENTED_EDGE ( 'NONE', *, *, #19418, .T. ) ;
#15159 = VERTEX_POINT ( 'NONE', #10897 ) ;
#15160 = CARTESIAN_POINT ( 'NONE',  ( 21.02850174869167788, 21.39790512250117871, 12.99999999999999467 ) ) ;
#15161 = CARTESIAN_POINT ( 'NONE',  ( 0.000000000000000000, 28.74062499938548854, 13.33755215474602984 ) ) ;
#15162 = CARTESIAN_POINT ( 'NONE',  ( 3.756430356250002323, -11.16877607737301403, 1.453124999385484228 ) ) ;
#15163 = ADVANCED_FACE ( 'NONE', ( #1225 ), #20990, .F. ) ;
#15164 = AXIS2_PLACEMENT_3D ( 'NONE', #22612, #6908, #24832 ) ;
#15165 = CARTESIAN_POINT ( 'NONE',  ( 3.756430356250002323, -11.16877607737301226, 4.265624999385481786 ) ) ;
#15166 =( NAMED_UNIT ( * ) SI_UNIT ( $, .STERADIAN. ) SOLID_ANGLE_UNIT ( ) );
#15167 = DIRECTION ( 'NONE',  ( 1.000000000000000000, 0.000000000000000000, 0.000000000000000000 ) ) ;
#15168 = FACE_OUTER_BOUND ( 'NONE', #24517, .T. ) ;
#15169 = LINE ( 'NONE', #3376, #11316 ) ;
#15170 = CARTESIAN_POINT ( 'NONE',  ( -3.756430356249996105, 28.02812499938548996, 6.831223922626973533 ) ) ;
#15171 = FACE_OUTER_BOUND ( 'NONE', #19562, .T. ) ;
#15172 = CARTESIAN_POINT ( 'NONE',  ( -25.99519186311192342, 0.5000000000000000000, 19.00000000000000000 ) ) ;
#15173 = DIRECTION ( 'NONE',  ( 0.000000000000000000, 1.000000000000000000, -0.000000000000000000 ) ) ;
#15174 = CYLINDRICAL_SURFACE ( 'NONE', #24285, 4.000000000000000000 ) ;
#15175 = CARTESIAN_POINT ( 'NONE',  ( -1.878215178125000939, -29.22812499938548569, 12.25316411605952283 ) ) ;
#15176 = CARTESIAN_POINT ( 'NONE',  ( 19.20116603387162613, 20.71691556172359938, 4.999999999999992006 ) ) ;
#15178 = EDGE_CURVE ( 'NONE', #21381, #14795, #15828, .T. ) ;
#15177 = CARTESIAN_POINT ( 'NONE',  ( -1.452785157361201396, 31.03863125411927371, -6.500000000000000000 ) ) ;
#15179 = DIRECTION ( 'NONE',  ( 1.000000000000000000, -0.000000000000000000, 0.000000000000000000 ) ) ;
#15180 = CARTESIAN_POINT ( 'NONE',  ( 20.14370442905180525, 20.14370442905174130, 12.99999999999999289 ) ) ;
#15181 = ORIENTED_EDGE ( 'NONE', *, *, #11148, .T. ) ;
#15182 = DIRECTION ( 'NONE',  ( -0.000000000000000000, 0.000000000000000000, 1.000000000000000000 ) ) ;
#15184 = VERTEX_POINT ( 'NONE', #7119 ) ;
#15183 = CARTESIAN_POINT ( 'NONE',  ( 0.000000000000000000, 0.000000000000000000, -6.500000000000000000 ) ) ;
#15185 = EDGE_LOOP ( 'NONE', ( #22569, #7448, #4228, #12449 ) ) ;
#15186 = ORIENTED_EDGE ( 'NONE', *, *, #10791, .F. ) ;
#15187 = ORIENTED_EDGE ( 'NONE', *, *, #18629, .F. ) ;
#15188 = ORIENTED_EDGE ( 'NONE', *, *, #22869, .F. ) ;
#15189 = FACE_OUTER_BOUND ( 'NONE', #14468, .T. ) ;
#15190 = DIRECTION ( 'NONE',  ( 0.000000000000000000, 0.000000000000000000, -1.000000000000000000 ) ) ;
#15191 = DIRECTION ( 'NONE',  ( 0.000000000000000000, 0.000000000000000000, 1.000000000000000000 ) ) ;
#15192 = CARTESIAN_POINT ( 'NONE',  ( 3.735045420075836212E-15, -4.662447845253954171, 0.7031249993854805647 ) ) ;
#15193 = CARTESIAN_POINT ( 'NONE',  ( -3.999999999999996003, -6.690598923241487306, 2.381249998770966769 ) ) ;
#15194 = CARTESIAN_POINT ( 'NONE',  ( 18.14379053194667790, 23.45618528786534895, 8.999999999999992895 ) ) ;
#15195 = CARTESIAN_POINT ( 'NONE',  ( 1.878215178125004048, 26.67812499938548498, 5.746835883940462963 ) ) ;
#15196 = PRESENTATION_LAYER_ASSIGNMENT (  '', '', ( #587 ) ) ;
#15197 = DIRECTION ( 'NONE',  ( 0.000000000000000000, -1.000000000000000000, 0.000000000000000000 ) ) ;
#15198 = CARTESIAN_POINT ( 'NONE',  ( 18.17706369300767832, 23.83391794249997631, 11.30940107675849404 ) ) ;
#15200 = EDGE_CURVE ( 'NONE', #21831, #9061, #7419, .T. ) ;
#15199 = CARTESIAN_POINT ( 'NONE',  ( 2.000000000000003997, -5.535898384862238508, 0.5250000000000011324 ) ) ;
#15201 = DIRECTION ( 'NONE',  ( 0.000000000000000000, 0.000000000000000000, 1.000000000000000000 ) ) ;
#15202 = CARTESIAN_POINT ( 'NONE',  ( 0.5000000000000000000, 0.000000000000000000, 19.50000000000000000 ) ) ;
#15203 = DIRECTION ( 'NONE',  ( 0.1253332335642980688, -0.9921147013144785420, 0.000000000000000000 ) ) ;
#15204 = CARTESIAN_POINT ( 'NONE',  ( -4.000000000000003553, -25.43124999877096926, 6.690598923241489970 ) ) ;
#15205 = CARTESIAN_POINT ( 'NONE',  ( -1.999999999999995781, -5.535898384862237620, 0.5437499987709683014 ) ) ;
#15206 = CARTESIAN_POINT ( 'NONE',  ( -3.999999999999999112, 25.18750000000000711, 6.690598923241487306 ) ) ;
#15207 = CARTESIAN_POINT ( 'NONE',  ( 2.000000000000003997, -5.535898384862238508, 4.068749998770968546 ) ) ;
#15208 = ORIENTED_EDGE ( 'NONE', *, *, #20352, .T. ) ;
#15209 = DIRECTION ( 'NONE',  ( 1.000000000000000000, 0.000000000000000000, 0.000000000000000000 ) ) ;
#15210 = ORIENTED_EDGE ( 'NONE', *, *, #20211, .T. ) ;
#15211 = EDGE_CURVE ( 'NONE', #10594, #20500, #4549, .T. ) ;
#15212 = VERTEX_POINT ( 'NONE', #3695 ) ;
#15213 = FACE_OUTER_BOUND ( 'NONE', #23178, .T. ) ;
#15214 = VERTEX_POINT ( 'NONE', #12055 ) ;
#15215 = CARTESIAN_POINT ( 'NONE',  ( -3.756430356250004099, -26.19062499938548783, 6.831223922626973533 ) ) ;
#15216 = VERTEX_POINT ( 'NONE', #2140 ) ;
#15217 = DIRECTION ( 'NONE',  ( -0.000000000000000000, -1.000000000000000000, -0.000000000000000000 ) ) ;
#15218 = ORIENTED_EDGE ( 'NONE', *, *, #25505, .F. ) ;
#15219 = CARTESIAN_POINT ( 'NONE',  ( -3.999999999999996003, 27.43750000000000000, 6.690598923241487306 ) ) ;
#15220 = CARTESIAN_POINT ( 'NONE',  ( 4.000000000000003553, 27.19374999877096855, 8.999999999999992895 ) ) ;
#15221 = DIRECTION ( 'NONE',  ( -0.000000000000000000, -0.000000000000000000, 1.000000000000000000 ) ) ;
#15222 = CARTESIAN_POINT ( 'NONE',  ( 28.34936733434196299, -12.78762572734067149, 1.000000000000000000 ) ) ;
#15223 = EDGE_CURVE ( 'NONE', #15567, #13481, #7834, .T. ) ;
#15224 = CARTESIAN_POINT ( 'NONE',  ( 16.34066823992098350, 21.65306299583965455, 11.16877607737301226 ) ) ;
#15225 = FACE_OUTER_BOUND ( 'NONE', #6127, .T. ) ;
#15226 = PRODUCT_DEFINITION_FORMATION_WITH_SPECIFIED_SOURCE ( 'ANY', '', #8177, .NOT_KNOWN. ) ;
#15227 = CARTESIAN_POINT ( 'NONE',  ( -3.999999999999996447, 26.57500000000000284, 8.999999999999992895 ) ) ;
#15228 = ADVANCED_FACE ( 'NONE', ( #21882 ), #19786, .F. ) ;
#15229 = CARTESIAN_POINT ( 'NONE',  ( 20.51057983692150444, 17.85438245896205700, 5.746835883940462963 ) ) ;
#15230 = LINE ( 'NONE', #5407, #23341 ) ;
#15231 = ORIENTED_EDGE ( 'NONE', *, *, #12704, .T. ) ;
#15233 = EDGE_CURVE ( 'NONE', #19968, #13187, #20037, .T. ) ;
#15232 = VERTEX_POINT ( 'NONE', #25548 ) ;
#15234 = CARTESIAN_POINT ( 'NONE',  ( 4.000000000000007105, 26.78124999877097423, 6.690598923241489970 ) ) ;
#15235 = CARTESIAN_POINT ( 'NONE',  ( 1.878215178124998497, -29.04062499938548569, 12.25316411605951927 ) ) ;
#15236 = EDGE_LOOP ( 'NONE', ( #16047, #2810, #7129, #6548 ) ) ;
#15237 = DIRECTION ( 'NONE',  ( 1.000000000000000000, 0.000000000000000000, 0.000000000000000000 ) ) ;
#15238 = CARTESIAN_POINT ( 'NONE',  ( 2.672651547586948120E-15, 27.84062499938548640, 13.33755215474602984 ) ) ;
#15239 = FACE_OUTER_BOUND ( 'NONE', #19737, .T. ) ;
#15240 = EDGE_CURVE ( 'NONE', #4730, #17275, #17471, .T. ) ;
#15241 = ORIENTED_EDGE ( 'NONE', *, *, #11269, .F. ) ;
#15242 = ORIENTED_EDGE ( 'NONE', *, *, #907, .T. ) ;
#15243 = CARTESIAN_POINT ( 'NONE',  ( 27.00874656207304980, 15.41874213889405176, -2.750000000000000000 ) ) ;
#15244 = DIRECTION ( 'NONE',  ( 0.000000000000000000, 0.000000000000000000, -1.000000000000000000 ) ) ;
#15245 = VERTEX_POINT ( 'NONE', #17962 ) ;
#15246 = CARTESIAN_POINT ( 'NONE',  ( -1.878215178125004048, -28.47812499938548569, 5.746835883940462963 ) ) ;
#15247 = CARTESIAN_POINT ( 'NONE',  ( 3.834746474454188013E-15, 26.01249999999999574, 4.999999999999992006 ) ) ;
#15248 = DIRECTION ( 'NONE',  ( 0.000000000000000000, 0.000000000000000000, 1.000000000000000000 ) ) ;
#15249 = LINE ( 'NONE', #13547, #22298 ) ;
#15250 = CARTESIAN_POINT ( 'NONE',  ( 3.756430356250000546, 29.15312499938548996, 11.16877607737301226 ) ) ;
#15251 = DIRECTION ( 'NONE',  ( 0.000000000000000000, 0.000000000000000000, 1.000000000000000000 ) ) ;
#15252 = APPLICATION_PROTOCOL_DEFINITION ( 'draft international standard', 'automotive_design', 1998, #15297 ) ;
#15253 = CYLINDRICAL_SURFACE ( 'NONE', #11673, 4.000000000000000000 ) ;
#15254 = DIRECTION ( 'NONE',  ( 0.000000000000000000, -1.000000000000000000, 0.000000000000000000 ) ) ;
#15255 = CARTESIAN_POINT ( 'NONE',  ( 3.756430356250002323, 26.90312499938548285, 11.16877607737301403 ) ) ;
#15256 = VECTOR ( 'NONE', #24430, 1000.000000000000000 ) ;
#15257 = CARTESIAN_POINT ( 'NONE',  ( -4.648177544792955347E-16, 27.08124999877097139, 12.99999999999999289 ) ) ;
#15258 = CARTESIAN_POINT ( 'NONE',  ( 21.16900926177230247, 15.51215501227985172, 6.690598923241489970 ) ) ;
#15259 = CARTESIAN_POINT ( 'NONE',  ( 18.57260154916842154, 18.57260154916834693, 4.662447845253954171 ) ) ;
#15260 =( BOUNDED_CURVE ( )  B_SPLINE_CURVE ( 2, ( #13251, #17702, #13386, #17320, #11666, #3686, #21608, #19390, #7243 ),
 .UNSPECIFIED., .F., .F. ) 
 B_SPLINE_CURVE_WITH_KNOTS ( ( 3, 2, 2, 2, 3 ),
 ( 0.1250000000000000000, 0.1333333333333333315, 0.1499999999999999944, 0.1666666666666666574, 0.1749999999999999889 ),
 .UNSPECIFIED. ) 
 CURVE ( )  GEOMETRIC_REPRESENTATION_ITEM ( )  RATIONAL_B_SPLINE_CURVE ( ( 0.9330127018922194093, 0.9330127018922194093, 1.000000000000000000, 0.8660254037844387076, 1.000000000000000000, 0.8660254037844387076, 1.000000000000000000, 0.9330127018922194093, 0.9330127018922194093 ) ) 
 REPRESENTATION_ITEM ( '' )  );
#15261 = CARTESIAN_POINT ( 'NONE',  ( 3.756430356250002323, 28.25312499938548427, 11.16877607737301226 ) ) ;
#15262 = CARTESIAN_POINT ( 'NONE',  ( 21.40018120162940818, 21.02622566956345196, 4.999999999999992006 ) ) ;
#15263 = CARTESIAN_POINT ( 'NONE',  ( 20.08404229395467055, 20.08404229395459240, 4.662447845253954171 ) ) ;
#15264 = CARTESIAN_POINT ( 'NONE',  ( 22.69370825783673951, 17.03685400834428521, 8.999999999999992895 ) ) ;
#15265 = EDGE_LOOP ( 'NONE', ( #16009, #791, #5998, #9291 ) ) ;
#15266 = CARTESIAN_POINT ( 'NONE',  ( 20.09951025522764922, 17.27108313048138655, 5.535898384862238508 ) ) ;
#15267 = CARTESIAN_POINT ( 'NONE',  ( 1.878215178125000939, 26.52812499938548285, 12.25316411605952283 ) ) ;
#15268 = CARTESIAN_POINT ( 'NONE',  ( -2.672651547586948120E-15, -28.62812499938548783, 13.33755215474602984 ) ) ;
#15269 = EDGE_CURVE ( 'NONE', #11648, #21178, #6055, .T. ) ;
#15271 = ORIENTED_EDGE ( 'NONE', *, *, #13065, .T. ) ;
#15270 = CARTESIAN_POINT ( 'NONE',  ( -0.5000000000000000000, -0.8660254037844387076, 19.50000000000000000 ) ) ;
#15272 = CARTESIAN_POINT ( 'NONE',  ( -1.878215178124995832, 26.75312499938548783, 5.746835883940462963 ) ) ;
#15273 =( BOUNDED_CURVE ( )  B_SPLINE_CURVE ( 2, ( #8958, #16932, #24901, #9202, #12862, #17192, #14960, #2931, #11149 ),
 .UNSPECIFIED., .F., .F. ) 
 B_SPLINE_CURVE_WITH_KNOTS ( ( 3, 2, 2, 2, 3 ),
 ( 0.7249999999999999778, 0.7333333333333332815, 0.7500000000000000000, 0.7666666666666667185, 0.7750000000000000222 ),
 .UNSPECIFIED. ) 
 CURVE ( )  GEOMETRIC_REPRESENTATION_ITEM ( )  RATIONAL_B_SPLINE_CURVE ( ( 0.9330127018922194093, 0.9330127018922194093, 1.000000000000000000, 0.8660254037844387076, 1.000000000000000000, 0.8660254037844387076, 1.000000000000000000, 0.9330127018922194093, 0.9330127018922194093 ) ) 
 REPRESENTATION_ITEM ( '' )  );
#15274 = EDGE_CURVE ( 'NONE', #11788, #21799, #4133, .T. ) ;
#15275 = EDGE_LOOP ( 'NONE', ( #6737, #4413, #24495, #4512 ) ) ;
#15276 = CARTESIAN_POINT ( 'NONE',  ( -1.878215178125004048, -27.91562499938548569, 5.746835883940462963 ) ) ;
#15277 = ORIENTED_EDGE ( 'NONE', *, *, #24207, .F. ) ;
#15278 = EDGE_LOOP ( 'NONE', ( #19851, #25781, #12307, #22215 ) ) ;
#15279 = CARTESIAN_POINT ( 'NONE',  ( 18.97414603143021594, 23.23826331710101556, 11.64163568064553544 ) ) ;
#15280 = CARTESIAN_POINT ( 'NONE',  ( 4.006172263299091013E-15, 28.96562499938548996, 4.662447845253954171 ) ) ;
#15281 = CARTESIAN_POINT ( 'NONE',  ( -3.756430356249996994, -8.999999999999992895, 4.528124999385485516 ) ) ;
#15282 = CYLINDRICAL_SURFACE ( 'NONE', #6361, 0.5000000000000004441 ) ;
#15283 = LINE ( 'NONE', #5337, #21346 ) ;
#15284 = CARTESIAN_POINT ( 'NONE',  ( 6.317933499823219279, -30.45149776762731975, -2.750000000000000000 ) ) ;
#15285 = CIRCLE ( 'NONE', #4831, 0.5000000000000011102 ) ;
#15286 = CARTESIAN_POINT ( 'NONE',  ( -0.2902671272941750868, -30.00000000000000355, 12.99999999999999112 ) ) ;
#15287 = CARTESIAN_POINT ( 'NONE',  ( -1.071796769724490117, 26.87634618820330701, 4.999999999999992895 ) ) ;
#15288 = CARTESIAN_POINT ( 'NONE',  ( -25.16042852506064165, 18.28012134629622309, -6.500000000000000000 ) ) ;
#15289 = CARTESIAN_POINT ( 'NONE',  ( 1.500000000000001776, -10.49999999999999289, 4.999999999999993783 ) ) ;
#15290 = CARTESIAN_POINT ( 'NONE',  ( -1.071796769724494558, -27.73615380933863861, 4.999999999999992895 ) ) ;
#15291 = CARTESIAN_POINT ( 'NONE',  ( 1.878215178124998497, -28.25312499938548427, 12.25316411605951927 ) ) ;
#15292 = DIRECTION ( 'NONE',  ( -0.4817536741017063306, 0.8763066800438685799, 0.000000000000000000 ) ) ;
#15293 = CARTESIAN_POINT ( 'NONE',  ( -23.96296185032681336, 19.82388608118453632, -6.500000000000000000 ) ) ;
#15294 = CARTESIAN_POINT ( 'NONE',  ( 2.000000000000000888, -12.46410161513774817, 4.424999999999998046 ) ) ;
#15295 = EDGE_CURVE ( 'NONE', #14528, #25775, #23454, .T. ) ;
#15296 = CARTESIAN_POINT ( 'NONE',  ( 3.469446951953614189E-15, 46.00000000000000000, 3.499999999999992895 ) ) ;
#15297 = APPLICATION_CONTEXT ( 'automotive_design' ) ;
#15298 = ORIENTED_EDGE ( 'NONE', *, *, #15604, .F. ) ;
#15299 = DIRECTION ( 'NONE',  ( -0.000000000000000000, 0.000000000000000000, 1.000000000000000000 ) ) ;
#15300 = DIRECTION ( 'NONE',  ( -3.552713678800501718E-15, 0.000000000000000000, 1.000000000000000000 ) ) ;
#15302 = EDGE_LOOP ( 'NONE', ( #20176, #10229, #20855, #5792 ) ) ;
#15301 = FACE_OUTER_BOUND ( 'NONE', #448, .T. ) ;
#15303 = EDGE_CURVE ( 'NONE', #6479, #10501, #4099, .T. ) ;
#15304 = ORIENTED_EDGE ( 'NONE', *, *, #10468, .F. ) ;
#15305 = ORIENTED_EDGE ( 'NONE', *, *, #4493, .T. ) ;
#15306 = ORIENTED_EDGE ( 'NONE', *, *, #8109, .F. ) ;
#15307 = ORIENTED_EDGE ( 'NONE', *, *, #16907, .T. ) ;
#15308 = FACE_OUTER_BOUND ( 'NONE', #722, .T. ) ;
#15309 = DIRECTION ( 'NONE',  ( -0.000000000000000000, -0.000000000000000000, -1.000000000000000000 ) ) ;
#15310 = CARTESIAN_POINT ( 'NONE',  ( 23.44808782266543901, 18.71365202105081949, 11.20140010723572566 ) ) ;
#15311 = EDGE_CURVE ( 'NONE', #24763, #21831, #9971, .T. ) ;
#15312 = CARTESIAN_POINT ( 'NONE',  ( -1.878215178124998497, -12.25316411605951927, 4.153124999385485516 ) ) ;
#15313 = CARTESIAN_POINT ( 'NONE',  ( 2.620986760973688460E-15, -13.61880215351699874, 2.081249998770966947 ) ) ;
#15314 = CARTESIAN_POINT ( 'NONE',  ( -3.756430356249996994, 25.92812499938548498, 8.999999999999992895 ) ) ;
#15315 = FACE_OUTER_BOUND ( 'NONE', #11582, .T. ) ;
#15316 = CARTESIAN_POINT ( 'NONE',  ( -11.91206721063010754, 28.72825533807145959, -6.500000000000000000 ) ) ;
#15317 = CARTESIAN_POINT ( 'NONE',  ( 4.000000000000001776, -11.30940107675849760, 0.8624999999999984901 ) ) ;
#15318 = DIRECTION ( 'NONE',  ( 0.000000000000000000, 0.000000000000000000, 1.000000000000000000 ) ) ;
#15319 = CARTESIAN_POINT ( 'NONE',  ( -16.16421332384701515, -26.25859848311253941, -6.500000000000000000 ) ) ;
#15320 = DIRECTION ( 'NONE',  ( -0.000000000000000000, -1.000000000000000000, -0.000000000000000000 ) ) ;
#15321 = CARTESIAN_POINT ( 'NONE',  ( -2.000000000000003997, -26.81874999877096855, 5.535898384862238508 ) ) ;
#15322 = CARTESIAN_POINT ( 'NONE',  ( 21.21320343559646915, 21.21320343559638744, 8.999999999999992895 ) ) ;
#15323 = CARTESIAN_POINT ( 'NONE',  ( -5.840899737312982509, 38.49999999999999289, 7.627451181685283466 ) ) ;
#15324 = DIRECTION ( 'NONE',  ( -0.000000000000000000, -1.000000000000000000, -0.000000000000000000 ) ) ;
#15325 = CARTESIAN_POINT ( 'NONE',  ( 4.000000000000003553, 25.00000000000000000, 8.999999999999992895 ) ) ;
#15326 = ORIENTED_EDGE ( 'NONE', *, *, #13164, .T. ) ;
#15327 = LINE ( 'NONE', #25141, #18361 ) ;
#15328 = ORIENTED_EDGE ( 'NONE', *, *, #18531, .F. ) ;
#15329 = EDGE_CURVE ( 'NONE', #21027, #6423, #3834, .T. ) ;
#15330 = ORIENTED_EDGE ( 'NONE', *, *, #21604, .F. ) ;
#15331 = DIRECTION ( 'NONE',  ( 1.000000000000000000, 0.000000000000000000, 0.000000000000000000 ) ) ;
#15332 = ORIENTED_EDGE ( 'NONE', *, *, #6840, .T. ) ;
#15333 = CARTESIAN_POINT ( 'NONE',  ( -2.672651547586948120E-15, -27.84062499938548640, 13.33755215474602984 ) ) ;
#15334 = ORIENTED_EDGE ( 'NONE', *, *, #12318, .F. ) ;
#15335 = CARTESIAN_POINT ( 'NONE',  ( -26.25859848311247902, 16.66421332384710752, -6.500000000000000000 ) ) ;
#15336 = EDGE_CURVE ( 'NONE', #8603, #19269, #13332, .T. ) ;
#15337 = ORIENTED_EDGE ( 'NONE', *, *, #11231, .F. ) ;
#15339 = CARTESIAN_POINT ( 'NONE',  ( 4.000000000000003553, 28.15000000000000213, 8.999999999999992895 ) ) ;
#15338 =( BOUNDED_CURVE ( )  B_SPLINE_CURVE ( 2, ( #24625, #1216, #6851, #833, #5154, #23069, #14834, #17047, #15091 ),
 .UNSPECIFIED., .F., .F. ) 
 B_SPLINE_CURVE_WITH_KNOTS ( ( 3, 2, 2, 2, 3 ),
 ( 0.5250000000000000222, 0.5333333333333333259, 0.5500000000000000444, 0.5666666666666666519, 0.5750000000000000666 ),
 .UNSPECIFIED. ) 
 CURVE ( )  GEOMETRIC_REPRESENTATION_ITEM ( )  RATIONAL_B_SPLINE_CURVE ( ( 0.9330127018922194093, 0.9330127018922194093, 1.000000000000000000, 0.8660254037844387076, 1.000000000000000000, 0.8660254037844387076, 1.000000000000000000, 0.9330127018922189652, 0.9330127018922194093 ) ) 
 REPRESENTATION_ITEM ( '' )  );
#15340 = EDGE_CURVE ( 'NONE', #25585, #13377, #25799, .T. ) ;
#15341 = CARTESIAN_POINT ( 'NONE',  ( 1.500000000000001776, -10.49999999999999289, 4.999999999999993783 ) ) ;
#15342 = FACE_OUTER_BOUND ( 'NONE', #20334, .T. ) ;
#15343 = CARTESIAN_POINT ( 'NONE',  ( 20.72498534553237093, 15.41259058961355954, 11.16877607737301226 ) ) ;
#15344 = FACE_OUTER_BOUND ( 'NONE', #24884, .T. ) ;
#15345 = CARTESIAN_POINT ( 'NONE',  ( -1.999999999999995781, 26.05000000000000071, 5.535898384862237620 ) ) ;
#15346 = CARTESIAN_POINT ( 'NONE',  ( 16.97706434298888212, 22.28945909890755317, 11.16877607737301048 ) ) ;
#15347 = CARTESIAN_POINT ( 'NONE',  ( -0.5000000000000000000, 0.8660254037844387076, 19.50000000000000000 ) ) ;
#15348 = ORIENTED_EDGE ( 'NONE', *, *, #12700, .F. ) ;
#15349 = VERTEX_POINT ( 'NONE', #19900 ) ;
#15350 = CARTESIAN_POINT ( 'NONE',  ( -4.000000000000000000, 27.41874999877096997, 8.999999999999992895 ) ) ;
#15351 = DIRECTION ( 'NONE',  ( 0.000000000000000000, 0.000000000000000000, 1.000000000000000000 ) ) ;
#15352 = ORIENTED_EDGE ( 'NONE', *, *, #5782, .F. ) ;
#15353 = CYLINDRICAL_SURFACE ( 'NONE', #1232, 31.10000000000000142 ) ;
#15354 = CARTESIAN_POINT ( 'NONE',  ( 1.878215178125000939, 27.87812499938548427, 12.25316411605952283 ) ) ;
#15355 = FACE_OUTER_BOUND ( 'NONE', #12565, .T. ) ;
#15356 = ORIENTED_EDGE ( 'NONE', *, *, #13506, .F. ) ;
#15357 = ORIENTED_EDGE ( 'NONE', *, *, #18499, .T. ) ;
#15358 = DIRECTION ( 'NONE',  ( 1.000000000000000000, 0.000000000000000000, 0.000000000000000000 ) ) ;
#15359 = EDGE_CURVE ( 'NONE', #21315, #13062, #24531, .T. ) ;
#15360 = VECTOR ( 'NONE', #9342, 1000.000000000000000 ) ;
#15361 = DIRECTION ( 'NONE',  ( -0.000000000000000000, 0.000000000000000000, 1.000000000000000000 ) ) ;
#15362 = ORIENTED_EDGE ( 'NONE', *, *, #13846, .F. ) ;
#15363 = CARTESIAN_POINT ( 'NONE',  ( 1.878215178124998497, -28.70312499938548356, 12.25316411605951927 ) ) ;
#15364 = DIRECTION ( 'NONE',  ( 0.000000000000000000, -0.000000000000000000, 1.000000000000000000 ) ) ;
#15365 = CARTESIAN_POINT ( 'NONE',  ( 1.878215178125003382, 27.46562499938548996, 5.746835883940462963 ) ) ;
#15366 = EDGE_CURVE ( 'NONE', #19882, #17641, #18484, .T. ) ;
#15367 =( BOUNDED_CURVE ( )  B_SPLINE_CURVE ( 2, ( #10302, #18294, #8617, #2463, #24173, #262, #4429, #14633, #8494 ),
 .UNSPECIFIED., .F., .F. ) 
 B_SPLINE_CURVE_WITH_KNOTS ( ( 3, 2, 2, 2, 3 ),
 ( 0.3250000000000000111, 0.3333333333333333148, 0.3499999999999999778, 0.3666666666666666408, 0.3750000000000000000 ),
 .UNSPECIFIED. ) 
 CURVE ( )  GEOMETRIC_REPRESENTATION_ITEM ( )  RATIONAL_B_SPLINE_CURVE ( ( 0.9330127018922194093, 0.9330127018922196314, 1.000000000000000000, 0.8660254037844387076, 1.000000000000000000, 0.8660254037844387076, 1.000000000000000000, 0.9330127018922194093, 0.9330127018922194093 ) ) 
 REPRESENTATION_ITEM ( '' )  );
#15368 = DIRECTION ( 'NONE',  ( 1.000000000000000000, 0.000000000000000000, 0.000000000000000000 ) ) ;
#15369 = CARTESIAN_POINT ( 'NONE',  ( -3.756430356249997882, 28.51562499938548711, 8.999999999999992895 ) ) ;
#15370 = CONTEXT_DEPENDENT_SHAPE_REPRESENTATION ( #6929, #12573 ) ;
#15371 = ADVANCED_FACE ( 'NONE', ( #18723 ), #10343, .T. ) ;
#15372 = CARTESIAN_POINT ( 'NONE',  ( -3.137519842735244810E-15, 26.91249999999999787, 4.999999999999991118 ) ) ;
#15373 = DIRECTION ( 'NONE',  ( 0.000000000000000000, 0.000000000000000000, 1.000000000000000000 ) ) ;
#15374 = VECTOR ( 'NONE', #7346, 1000.000000000000000 ) ;
#15375 = CARTESIAN_POINT ( 'NONE',  ( -1.878215178124998497, 27.24062499938548498, 12.25316411605951927 ) ) ;
#15376 = CARTESIAN_POINT ( 'NONE',  ( -2.645323980344223447, -29.88371542788442881, 5.988343842124890237 ) ) ;
#15377 = CARTESIAN_POINT ( 'NONE',  ( 20.72043839702256207, 20.72043839702248036, 4.662447845253954171 ) ) ;
#15378 = CARTESIAN_POINT ( 'NONE',  ( 23.08495422774248240, 17.77255947182365503, 6.831223922626973533 ) ) ;
#15379 = CARTESIAN_POINT ( 'NONE',  ( 17.70860545047158396, 20.53703257521770453, 12.46410161513774639 ) ) ;
#15380 = DIRECTION ( 'NONE',  ( 1.000000000000000000, 0.000000000000000000, -0.000000000000000000 ) ) ;
#15381 = DIRECTION ( 'NONE',  ( 1.000000000000000000, 0.000000000000000000, -0.000000000000000000 ) ) ;
#15382 = CARTESIAN_POINT ( 'NONE',  ( 20.00676625532608455, 17.35056887736664422, 12.25316411605952283 ) ) ;
#15383 = DIRECTION ( 'NONE',  ( -0.000000000000000000, 0.000000000000000000, 1.000000000000000000 ) ) ;
#15384 = ORIENTED_EDGE ( 'NONE', *, *, #12733, .F. ) ;
#15385 = CARTESIAN_POINT ( 'NONE',  ( 2.620986760973688460E-15, 26.18124999877096926, 13.61880215351699874 ) ) ;
#15387 = EDGE_CURVE ( 'NONE', #10075, #11934, #2775, .T. ) ;
#15386 = CARTESIAN_POINT ( 'NONE',  ( -3.999999999999997335, 29.70624999877097139, 11.30940107675849404 ) ) ;
#15388 = CARTESIAN_POINT ( 'NONE',  ( -3.735045420075836212E-15, -29.30312499938548498, 4.662447845253954171 ) ) ;
#15390 = ORIENTED_EDGE ( 'NONE', *, *, #7117, .F. ) ;
#15389 = PLANE ( 'NONE',  #10412 ) ;
#15391 = CARTESIAN_POINT ( 'NONE',  ( -1.878215178124998497, 26.45312499938548711, 12.25316411605951927 ) ) ;
#15392 = ORIENTED_EDGE ( 'NONE', *, *, #19751, .T. ) ;
#15393 = CARTESIAN_POINT ( 'NONE',  ( -2.672651547586948120E-15, -28.17812499938548143, 13.33755215474602984 ) ) ;
#15394 = VERTEX_POINT ( 'NONE', #14308 ) ;
#15395 = VERTEX_POINT ( 'NONE', #4350 ) ;
#15396 = DIRECTION ( 'NONE',  ( 0.000000000000000000, 0.000000000000000000, 1.000000000000000000 ) ) ;
#15397 = CARTESIAN_POINT ( 'NONE',  ( 1.878215178125003382, 29.37812499938548783, 5.746835883940462963 ) ) ;
#15398 = AXIS2_PLACEMENT_3D ( 'NONE', #2745, #10707, #9140 ) ;
#15399 = CIRCLE ( 'NONE', #4520, 31.10000000000000142 ) ;
#15400 = CARTESIAN_POINT ( 'NONE',  ( 3.756430356250003211, -6.831223922626973533, 0.6281249993854786107 ) ) ;
#15401 = ADVANCED_FACE ( 'NONE', ( #22271 ), #815, .F. ) ;
#15402 = AXIS2_PLACEMENT_3D ( 'NONE', #2844, #12669, #6902 ) ;
#15403 = AXIS2_PLACEMENT_3D ( 'NONE', #23294, #1588, #4777 ) ;
#15404 = CARTESIAN_POINT ( 'NONE',  ( 4.000000000000003553, 29.03124999877096712, 6.690598923241489970 ) ) ;
#15405 =( NAMED_UNIT ( * ) PLANE_ANGLE_UNIT ( ) SI_UNIT ( $, .RADIAN. ) );
#15406 = ADVANCED_FACE ( 'NONE', ( #14163 ), #20169, .F. ) ;
#15407 = FACE_OUTER_BOUND ( 'NONE', #9261, .T. ) ;
#15408 = EDGE_CURVE ( 'NONE', #16617, #21696, #14539, .T. ) ;
#15409 = CARTESIAN_POINT ( 'NONE',  ( 4.000000000000002665, 26.76250000000000284, 11.30940107675849760 ) ) ;
#15410 = DIRECTION ( 'NONE',  ( 0.000000000000000000, -0.000000000000000000, 1.000000000000000000 ) ) ;
#15411 = CARTESIAN_POINT ( 'NONE',  ( 4.000000000000003553, 28.60000000000000142, 8.999999999999992895 ) ) ;
#15412 = B_SPLINE_CURVE_WITH_KNOTS ( 'NONE', 3,
 ( #20853, #10908, #1105, #18904, #22703, #16821, #17064, #4783, #12757, #9353 ),
 .UNSPECIFIED., .F., .F.,
 ( 4, 2, 2, 2, 4 ),
 ( 0.01251976117704806969, 0.01338929815772730951, 0.01425883513840654759, 0.01512837211908578741, 0.01599790909976502723 ),
 .UNSPECIFIED. ) ;
#15413 = CARTESIAN_POINT ( 'NONE',  ( 4.000000000000001776, 25.80624999877096926, 11.30940107675849760 ) ) ;
#15414 = CARTESIAN_POINT ( 'NONE',  ( 26.49999999999999645, -0.5000000000000000000, 19.00000000000000000 ) ) ;
#15415 = CARTESIAN_POINT ( 'NONE',  ( 15.63147928073609982, 21.28833353022841379, 11.30940107675849404 ) ) ;
#15416 = ORIENTED_EDGE ( 'NONE', *, *, #19096, .T. ) ;
#15417 = CARTESIAN_POINT ( 'NONE',  ( 1.626862140677534194E-14, 27.58750000000000213, 12.99999999999999289 ) ) ;
#15418 = DIRECTION ( 'NONE',  ( 0.000000000000000000, 0.000000000000000000, 1.000000000000000000 ) ) ;
#15419 =( BOUNDED_CURVE ( )  B_SPLINE_CURVE ( 2, ( #16573, #24532, #2704, #10933, #16317, #10794, #22844, #8712, #10665, #18786, #874, #18656, #16844, #20877, #21018, #15517, #9484, #11318, #11062, #25315, #22972, #5307, #3341, #5434, #23223, #7279, #19163, #23346, #7395, #17086, #19422, #18924, #19040, #25058, #3095, #13039, #13427, #14993, #1515, #25201, #1123, #21399, #19298, #17465, #9098, #23486, #1255, #15255, #25436, #17229, #7520, #1397, #7148, #15138, #9370, #5189, #15375, #13285, #1008, #23107, #5060, #21517, #17351, #3478, #11451, #13167, #21136, #3209, #21261, #11179, #9240, #5572, #13552, #3599, #8985, #16962, #24929, #7008, #6441, #10100, #1641, #18483, #14161, #8407, #2137, #6309, #14304, #22129, #24483, #22268, #20166, #18219, #16523, #7660, #2266, #25574, #14035, #178, #14544, #19539, #437, #12445, #17597, #24090, #572, #16395, #14426, #22387, #4217, #12323, #15643, #4347, #12052, #20032, #6563, #10340, #24222, #20291, #24364, #16253, #301 ),
 .UNSPECIFIED., .F., .F. ) 
 B_SPLINE_CURVE_WITH_KNOTS ( ( 3, 2, 2, 2, 2, 2, 2, 2, 2, 2, 2, 2, 2, 2, 2, 2, 2, 2, 2, 2, 2, 2, 2, 2, 2, 2, 2, 2, 2, 2, 2, 2, 2, 2, 2, 2, 2, 2, 2, 2, 2, 2, 2, 2, 2, 2, 2, 2, 2, 2, 2, 2, 2, 2, 2, 2, 2, 2, 2, 2, 3 ),
 ( 0.000000000000000000, 0.01666666666666666644, 0.03333333333333333287, 0.05000000000000000278, 0.06666666666666666574, 0.08333333333333332871, 0.1000000000000000056, 0.1166666666666666685, 0.1333333333333333315, 0.1499999999999999944, 0.1666666666666666574, 0.1833333333333333204, 0.2000000000000000111, 0.2166666666666666741, 0.2333333333333333370, 0.2500000000000000000, 0.2666666666666666630, 0.2833333333333333259, 0.2999999999999999889, 0.3166666666666666519, 0.3333333333333333148, 0.3499999999999999778, 0.3666666666666666408, 0.3833333333333333592, 0.4000000000000000222, 0.4166666666666666852, 0.4333333333333333481, 0.4500000000000000111, 0.4666666666666666741, 0.4833333333333333370, 0.5000000000000000000, 0.5166666666666667185, 0.5333333333333333259, 0.5500000000000000444, 0.5666666666666666519, 0.5833333333333333703, 0.5999999999999999778, 0.6166666666666666963, 0.6333333333333333037, 0.6500000000000000222, 0.6666666666666666297, 0.6833333333333333481, 0.6999999999999999556, 0.7166666666666666741, 0.7333333333333332815, 0.7500000000000000000, 0.7666666666666667185, 0.7833333333333333259, 0.8000000000000000444, 0.8166666666666666519, 0.8333333333333333703, 0.8499999999999999778, 0.8666666666666666963, 0.8833333333333333037, 0.9000000000000000222, 0.9166666666666666297, 0.9333333333333333481, 0.9499999999999999556, 0.9666666666666666741, 0.9833333333333332815, 1.000000000000000000 ),
 .UNSPECIFIED. ) 
 CURVE ( )  GEOMETRIC_REPRESENTATION_ITEM ( )  RATIONAL_B_SPLINE_CURVE ( ( 1.000000000000000000, 0.8660254037844387076, 1.000000000000000000, 0.8660254037844387076, 1.000000000000000000, 0.8660254037844387076, 1.000000000000000000, 0.8660254037844387076, 1.000000000000000000, 0.8660254037844387076, 1.000000000000000000, 0.8660254037844387076, 1.000000000000000000, 0.8660254037844387076, 1.000000000000000000, 0.8660254037844387076, 1.000000000000000000, 0.8660254037844387076, 1.000000000000000000, 0.8660254037844387076, 1.000000000000000000, 0.8660254037844387076, 1.000000000000000000, 0.8660254037844387076, 1.000000000000000000, 0.8660254037844387076, 1.000000000000000000, 0.8660254037844387076, 1.000000000000000000, 0.8660254037844387076, 1.000000000000000000, 0.8660254037844387076, 1.000000000000000000, 0.8660254037844387076, 1.000000000000000000, 0.8660254037844387076, 1.000000000000000000, 0.8660254037844387076, 1.000000000000000000, 0.8660254037844387076, 1.000000000000000000, 0.8660254037844387076, 1.000000000000000000, 0.8660254037844387076, 1.000000000000000000, 0.8660254037844387076, 1.000000000000000000, 0.8660254037844387076, 1.000000000000000000, 0.8660254037844387076, 1.000000000000000000, 0.8660254037844387076, 1.000000000000000000, 0.8660254037844387076, 1.000000000000000000, 0.8660254037844387076, 1.000000000000000000, 0.8660254037844387076, 1.000000000000000000, 0.8660254037844387076, 1.000000000000000000, 0.8660254037844387076, 1.000000000000000000, 0.8660254037844387076, 1.000000000000000000, 0.8660254037844387076, 1.000000000000000000, 0.8660254037844387076, 1.000000000000000000, 0.8660254037844387076, 1.000000000000000000, 0.8660254037844387076, 1.000000000000000000, 0.8660254037844387076, 1.000000000000000000, 0.8660254037844387076, 1.000000000000000000, 0.8660254037844387076, 1.000000000000000000, 0.8660254037844387076, 1.000000000000000000, 0.8660254037844387076, 1.000000000000000000, 0.8660254037844387076, 1.000000000000000000, 0.8660254037844387076, 1.000000000000000000, 0.8660254037844387076, 1.000000000000000000, 0.8660254037844387076, 1.000000000000000000, 0.8660254037844387076, 1.000000000000000000, 0.8660254037844387076, 1.000000000000000000, 0.8660254037844387076, 1.000000000000000000, 0.8660254037844387076, 1.000000000000000000, 0.8660254037844387076, 1.000000000000000000, 0.8660254037844387076, 1.000000000000000000, 0.8660254037844387076, 1.000000000000000000, 0.8660254037844387076, 1.000000000000000000, 0.8660254037844387076, 1.000000000000000000, 0.8660254037844387076, 1.000000000000000000, 0.8660254037844387076, 1.000000000000000000, 0.8660254037844387076, 1.000000000000000000, 0.8660254037844387076, 1.000000000000000000, 0.8660254037844387076, 1.000000000000000000, 0.8660254037844387076, 1.000000000000000000 ) ) 
 REPRESENTATION_ITEM ( '' )  );
#15420 = DIRECTION ( 'NONE',  ( 1.000000000000000000, 0.000000000000000000, 0.000000000000000000 ) ) ;
#15421 = CARTESIAN_POINT ( 'NONE',  ( 21.16900926177230247, 15.51215501227985172, 6.690598923241489970 ) ) ;
#15422 = CIRCLE ( 'NONE', #25430, 0.5000000000000007772 ) ;
#15423 = CARTESIAN_POINT ( 'NONE',  ( -2.000000000000000888, -28.52500000000000213, 12.46410161513774817 ) ) ;
#15425 = ORIENTED_EDGE ( 'NONE', *, *, #23557, .F. ) ;
#15424 = AXIS2_PLACEMENT_3D ( 'NONE', #23840, #1998, #5544 ) ;
#15426 = CARTESIAN_POINT ( 'NONE',  ( -3.397863563850083146, -30.85476721088024021, -6.500000000000000000 ) ) ;
#15427 = CARTESIAN_POINT ( 'NONE',  ( -20.20656826142300133, -23.64116323484216053, -2.750000000000000000 ) ) ;
#15429 = ORIENTED_EDGE ( 'NONE', *, *, #13144, .F. ) ;
#15428 = DIRECTION ( 'NONE',  ( 0.000000000000000000, 0.000000000000000000, 1.000000000000000000 ) ) ;
#15430 = ORIENTED_EDGE ( 'NONE', *, *, #13633, .F. ) ;
#15432 = ORIENTED_EDGE ( 'NONE', *, *, #2294, .F. ) ;
#15431 = AXIS2_PLACEMENT_3D ( 'NONE', #24194, #14275, #9819 ) ;
#15433 = ORIENTED_EDGE ( 'NONE', *, *, #11349, .F. ) ;
#15434 = ORIENTED_EDGE ( 'NONE', *, *, #22318, .T. ) ;
#15435 = DIRECTION ( 'NONE',  ( 0.000000000000000000, 0.000000000000000000, 1.000000000000000000 ) ) ;
#15436 = DIRECTION ( 'NONE',  ( -0.1253332335642912687, 0.9921147013144795412, 0.000000000000000000 ) ) ;
#15437 = CARTESIAN_POINT ( 'NONE',  ( -1.878215178124998275, 25.44062499938549138, 12.25316411605951927 ) ) ;
#15438 = VECTOR ( 'NONE', #14477, 1000.000000000000000 ) ;
#15439 = CIRCLE ( 'NONE', #6247, 31.10000000000000142 ) ;
#15440 = CARTESIAN_POINT ( 'NONE',  ( 2.672651547586948120E-15, -13.33755215474602984, 3.178124999385481431 ) ) ;
#15441 = CARTESIAN_POINT ( 'NONE',  ( 4.000000000000003553, -6.690598923241489970, 0.8812499987709634386 ) ) ;
#15442 = ADVANCED_FACE ( 'NONE', ( #2270 ), #6444, .T. ) ;
#15443 = CARTESIAN_POINT ( 'NONE',  ( 3.756430356250004099, 27.54062499938548569, 6.831223922626973533 ) ) ;
#15445 = ADVANCED_FACE ( 'NONE', ( #18344 ), #4754, .F. ) ;
#15444 = CIRCLE ( 'NONE', #5814, 0.4999999999999999445 ) ;
#15446 = CARTESIAN_POINT ( 'NONE',  ( 4.000000000000003553, -8.999999999999992895, 3.993749998770966592 ) ) ;
#15447 = CARTESIAN_POINT ( 'NONE',  ( 4.000000000000001776, 29.69687499938548925, 8.999999999999992895 ) ) ;
#15448 = VECTOR ( 'NONE', #14169, 1000.000000000000000 ) ;
#15449 = CARTESIAN_POINT ( 'NONE',  ( -1.999999999999998224, -12.46410161513774639, 1.199999999999999734 ) ) ;
#15450 = APPLICATION_CONTEXT ( 'automotive_design' ) ;
#15451 = CARTESIAN_POINT ( 'NONE',  ( 10.08469938919477649, -29.41953157733097868, 1.000000000000000000 ) ) ;
#15452 = DIRECTION ( 'NONE',  ( -0.000000000000000000, -1.000000000000000000, -0.000000000000000000 ) ) ;
#15453 = CARTESIAN_POINT ( 'NONE',  ( 0.000000000000000000, 0.000000000000000000, -6.500000000000000000 ) ) ;
#15454 = CARTESIAN_POINT ( 'NONE',  ( 3.999999999999997335, -27.45624999877096784, 11.30940107675849404 ) ) ;
#15455 = ADVANCED_FACE ( 'NONE', ( #574 ), #20693, .T. ) ;
#15456 = CARTESIAN_POINT ( 'NONE',  ( -3.756430356249996994, -8.999999999999992895, 4.528124999385485516 ) ) ;
#15457 = CARTESIAN_POINT ( 'NONE',  ( 0.000000000000000000, 0.000000000000000000, -6.500000000000000000 ) ) ;
#15458 = AXIS2_PLACEMENT_3D ( 'NONE', #8569, #8302, #24001 ) ;
#15459 = CARTESIAN_POINT ( 'NONE',  ( 3.469446951953614189E-15, -8.999999999999992895, 18.00000000000000000 ) ) ;
#15460 = CARTESIAN_POINT ( 'NONE',  ( -4.000000000000003553, -25.90000000000000213, 8.999999999999992895 ) ) ;
#15461 = ORIENTED_EDGE ( 'NONE', *, *, #7545, .F. ) ;
#15462 = CARTESIAN_POINT ( 'NONE',  ( 22.32573188046920265, 21.65113613650335367, 1.000000000000000000 ) ) ;
#15463 = ORIENTED_EDGE ( 'NONE', *, *, #22508, .T. ) ;
#15464 = AXIS2_PLACEMENT_3D ( 'NONE', #11953, #8050, #17851 ) ;
#15465 = ORIENTED_EDGE ( 'NONE', *, *, #7804, .T. ) ;
#15466 = DIRECTION ( 'NONE',  ( -0.000000000000000000, -0.000000000000000000, 1.000000000000000000 ) ) ;
#15467 = ORIENTED_EDGE ( 'NONE', *, *, #9613, .T. ) ;
#15468 = CARTESIAN_POINT ( 'NONE',  ( -2.672651547586948120E-15, -26.94062499938548783, 13.33755215474602984 ) ) ;
#15469 = ORIENTED_EDGE ( 'NONE', *, *, #20875, .T. ) ;
#15470 = CARTESIAN_POINT ( 'NONE',  ( -3.999999999999995559, 28.78750000000000142, 6.690598923241487306 ) ) ;
#15471 = CIRCLE ( 'NONE', #840, 27.10000000000000142 ) ;
#15472 = EDGE_LOOP ( 'NONE', ( #10265, #18196, #7711, #4064, #2414, #3764, #24199, #22895 ) ) ;
#15473 = CARTESIAN_POINT ( 'NONE',  ( -3.999999999999996447, 28.37500000000000000, 8.999999999999992895 ) ) ;
#15474 = DIRECTION ( 'NONE',  ( 1.000000000000000000, 0.000000000000000000, 0.000000000000000000 ) ) ;
#15475 = VECTOR ( 'NONE', #6988, 1000.000000000000000 ) ;
#15476 = CARTESIAN_POINT ( 'NONE',  ( -1.878215178124995832, -5.746835883940462963, 0.8531249993854843616 ) ) ;
#15477 = DIRECTION ( 'NONE',  ( 1.000000000000000000, 0.000000000000000000, 0.000000000000000000 ) ) ;
#15478 = CARTESIAN_POINT ( 'NONE',  ( 19.18020767368691182, 21.83640505164621004, 5.746835883940462963 ) ) ;
#15479 = EDGE_CURVE ( 'NONE', #25112, #11742, #19304, .T. ) ;
#15480 = VECTOR ( 'NONE', #4316, 1000.000000000000000 ) ;
#15481 = DIRECTION ( 'NONE',  ( 0.000000000000000000, 0.000000000000000000, -1.000000000000000000 ) ) ;
#15482 = EDGE_CURVE ( 'NONE', #16373, #3186, #2852, .T. ) ;
#15483 = CARTESIAN_POINT ( 'NONE',  ( -1.999999999999998224, 25.30000000000000426, 12.46410161513774639 ) ) ;
#15484 = VECTOR ( 'NONE', #11586, 1000.000000000000000 ) ;
#15485=STYLED_ITEM('',(#25928),#22659);
#15486 = CARTESIAN_POINT ( 'NONE',  ( 16.60583328286593741, 21.91822803878461912, 6.831223922626973533 ) ) ;
#15487 = CARTESIAN_POINT ( 'NONE',  ( 0.000000000000000000, 0.000000000000000000, -6.500000000000000000 ) ) ;
#15488 = ORIENTED_EDGE ( 'NONE', *, *, #15761, .T. ) ;
#15489 = EDGE_LOOP ( 'NONE', ( #2299, #16562, #14340, #3810 ) ) ;
#15490 = CARTESIAN_POINT ( 'NONE',  ( 2.000000000000000000, 28.01874999877097139, 12.46410161513774817 ) ) ;
#15491 = CARTESIAN_POINT ( 'NONE',  ( -1.878215178125000939, -28.66562499938548569, 12.25316411605952283 ) ) ;
#15492 = EDGE_CURVE ( 'NONE', #8456, #16614, #11279, .T. ) ;
#15493 = ORIENTED_EDGE ( 'NONE', *, *, #7069, .F. ) ;
#15494 = CARTESIAN_POINT ( 'NONE',  ( 0.000000000000000000, 0.000000000000000000, -6.500000000000000000 ) ) ;
#15495 = CIRCLE ( 'NONE', #16310, 6.000000000000000000 ) ;
#15496 = CARTESIAN_POINT ( 'NONE',  ( 2.672651547586948120E-15, 28.29062499938548569, 13.33755215474602984 ) ) ;
#15497 = DIRECTION ( 'NONE',  ( 0.000000000000000000, 0.000000000000000000, 1.000000000000000000 ) ) ;
#15498 = ORIENTED_EDGE ( 'NONE', *, *, #14019, .T. ) ;
#15499 = VERTEX_POINT ( 'NONE', #2902 ) ;
#15500 = AXIS2_PLACEMENT_3D ( 'NONE', #5064, #19167, #5311 ) ;
#15501 = AXIS2_PLACEMENT_3D ( 'NONE', #4211, #12439, #22656 ) ;
#15502 = CARTESIAN_POINT ( 'NONE',  ( 28.14012133169314822, -13.24173596767388794, -6.500000000000000000 ) ) ;
#15503 = VERTEX_POINT ( 'NONE', #11131 ) ;
#15504 = AXIS2_PLACEMENT_3D ( 'NONE', #2045, #19942, #22309 ) ;
#15505 = CYLINDRICAL_SURFACE ( 'NONE', #24358, 4.000000000000000000 ) ;
#15506 = CARTESIAN_POINT ( 'NONE',  ( -3.756430356249997882, 25.85312499938548925, 11.16877607737301226 ) ) ;
#15507 = CARTESIAN_POINT ( 'NONE',  ( 1.878215178125003382, 27.01562499938548711, 5.746835883940462963 ) ) ;
#15508 = VECTOR ( 'NONE', #14509, 1000.000000000000000 ) ;
#15509 = CARTESIAN_POINT ( 'NONE',  ( -0.4999838450259764255, -31.09598070739550124, -6.500000000000000000 ) ) ;
#15510 = CARTESIAN_POINT ( 'NONE',  ( 8.012344526598182026E-15, 26.91250000000000497, 4.381197846482986158 ) ) ;
#15511 = VECTOR ( 'NONE', #17187, 1000.000000000000000 ) ;
#15512 = CARTESIAN_POINT ( 'NONE',  ( -3.756430356249997882, 27.65312499938548640, 11.16877607737301226 ) ) ;
#15513 = DIRECTION ( 'NONE',  ( 0.000000000000000000, 0.000000000000000000, 1.000000000000000000 ) ) ;
#15514 = CIRCLE ( 'NONE', #6751, 31.10000000000000142 ) ;
#15515 = CIRCLE ( 'NONE', #4232, 31.10000000000000142 ) ;
#15516 = CARTESIAN_POINT ( 'NONE',  ( -28.41604871112448549, 11.44867358849382910, -6.500000000000000000 ) ) ;
#15517 = CARTESIAN_POINT ( 'NONE',  ( 3.735045420075836212E-15, 25.70312499938548001, 4.662447845253954171 ) ) ;
#15518 = ADVANCED_FACE ( 'NONE', ( #17032 ), #5255, .F. ) ;
#15519 = CARTESIAN_POINT ( 'NONE',  ( 0.000000000000000000, 0.000000000000000000, 1.000000000000000000 ) ) ;
#15520 = CARTESIAN_POINT ( 'NONE',  ( 16.91752973988819164, 22.57438398938050028, 8.999999999999992895 ) ) ;
#15521 = CARTESIAN_POINT ( 'NONE',  ( 21.67730602587931088, 19.02110864791986344, 12.25316411605952283 ) ) ;
#15522 = DIRECTION ( 'NONE',  ( 0.000000000000000000, 0.000000000000000000, 1.000000000000000000 ) ) ;
#15523 = CARTESIAN_POINT ( 'NONE',  ( 3.735045420075836212E-15, 29.30312499938548498, 4.662447845253954171 ) ) ;
#15524 = VECTOR ( 'NONE', #14088, 1000.000000000000000 ) ;
#15525 = DIRECTION ( 'NONE',  ( 0.000000000000000000, 0.000000000000000000, 1.000000000000000000 ) ) ;
#15526 = CARTESIAN_POINT ( 'NONE',  ( 21.06742642710591440, 18.41122904914646341, 5.746835883940462963 ) ) ;
#15527 = LINE ( 'NONE', #17607, #3350 ) ;
#15528 = ORIENTED_EDGE ( 'NONE', *, *, #21124, .T. ) ;
#15529 = CARTESIAN_POINT ( 'NONE',  ( 4.000000000000003553, 26.78124999877097068, 6.690598923241489970 ) ) ;
#15530 = CARTESIAN_POINT ( 'NONE',  ( -4.000000000000003553, -26.35000000000000142, 8.999999999999992895 ) ) ;
#15532 = ORIENTED_EDGE ( 'NONE', *, *, #9750, .F. ) ;
#15531 = FACE_BOUND ( 'NONE', #8215, .T. ) ;
#15533 = CARTESIAN_POINT ( 'NONE',  ( 3.735045420075836212E-15, 27.16562499938547859, 4.662447845253954171 ) ) ;
#15534 = DIRECTION ( 'NONE',  ( -0.000000000000000000, -0.000000000000000000, 1.000000000000000000 ) ) ;
#15535 = CARTESIAN_POINT ( 'NONE',  ( -25.16843286583315731, 6.741346781237202102, 20.00001200000000168 ) ) ;
#15536 = CARTESIAN_POINT ( 'NONE',  ( 4.000000000000003553, 26.29374999877096997, 8.999999999999992895 ) ) ;
#15537 = EDGE_LOOP ( 'NONE', ( #9572, #23318, #15153, #13307 ) ) ;
#15538 = ORIENTED_EDGE ( 'NONE', *, *, #20182, .T. ) ;
#15539 =( LENGTH_UNIT ( ) NAMED_UNIT ( * ) SI_UNIT ( .MILLI., .METRE. ) );
#15540 = AXIS2_PLACEMENT_3D ( 'NONE', #6273, #14264, #7842 ) ;
#15541 = CARTESIAN_POINT ( 'NONE',  ( -3.756430356249996105, 26.22812499938548569, 6.831223922626973533 ) ) ;
#15542 = CARTESIAN_POINT ( 'NONE',  ( -3.756430356249996994, -8.999999999999992895, 1.265624999385484006 ) ) ;
#15543 = CIRCLE ( 'NONE', #23468, 0.5000000000000003331 ) ;
#15544 = CARTESIAN_POINT ( 'NONE',  ( 1.878215178125004048, -5.746835883940462963, 3.928124999385485872 ) ) ;
#15545 = CARTESIAN_POINT ( 'NONE',  ( 25.98730014090430274, -17.08421000182786997, -6.500000000000000000 ) ) ;
#15546 = CARTESIAN_POINT ( 'NONE',  ( 3.834746474454188013E-15, 26.01249999999999574, 4.999999999999992006 ) ) ;
#15547 = AXIS2_PLACEMENT_3D ( 'NONE', #23033, #7449, #1449 ) ;
#15548 = DIRECTION ( 'NONE',  ( 0.000000000000000000, 0.000000000000000000, 1.000000000000000000 ) ) ;
#15549 = CARTESIAN_POINT ( 'NONE',  ( -1.999999999999995781, 26.50000000000000355, 5.535898384862237620 ) ) ;
#15550 = CARTESIAN_POINT ( 'NONE',  ( 0.000000000000000000, 0.000000000000000000, -6.500000000000000000 ) ) ;
#15551 = CARTESIAN_POINT ( 'NONE',  ( -3.999999999999996447, -8.999999999999992895, 1.968749998770967569 ) ) ;
#15552 = CARTESIAN_POINT ( 'NONE',  ( -27.25313774936430633, -14.98253926456308172, -6.500000000000000000 ) ) ;
#15553 = ORIENTED_EDGE ( 'NONE', *, *, #10098, .T. ) ;
#15554 = CARTESIAN_POINT ( 'NONE',  ( -4.000000000000001776, -27.60624999877096641, 11.30940107675849760 ) ) ;
#15555 = CARTESIAN_POINT ( 'NONE',  ( -30.54913349766228592, -5.827558883615738594, 1.000000000000000000 ) ) ;
#15556 = CARTESIAN_POINT ( 'NONE',  ( -3.756430356249996994, 27.27812499938548640, 8.999999999999992895 ) ) ;
#15557 = AXIS2_PLACEMENT_3D ( 'NONE', #9135, #11217, #24711 ) ;
#15559 = ADVANCED_FACE ( 'NONE', ( #10869 ), #6959, .F. ) ;
#15558 = FACE_OUTER_BOUND ( 'NONE', #4294, .T. ) ;
#15560 = CARTESIAN_POINT ( 'NONE',  ( 3.000000000000003997, -8.999999999999992895, 0.000000000000000000 ) ) ;
#15561 = DIRECTION ( 'NONE',  ( -0.000000000000000000, -1.000000000000000000, -0.000000000000000000 ) ) ;
#15562 = VERTEX_POINT ( 'NONE', #14938 ) ;
#15563 = DIRECTION ( 'NONE',  ( 0.4257792915650852050, 0.9048270524660135816, 0.000000000000000000 ) ) ;
#15565 = ORIENTED_EDGE ( 'NONE', *, *, #14187, .F. ) ;
#15564 = CARTESIAN_POINT ( 'NONE',  ( -8.831537335106614961E-15, -26.23749999999999716, 12.99999999999999112 ) ) ;
#15566 = EDGE_CURVE ( 'NONE', #8668, #10289, #14955, .T. ) ;
#15567 = VERTEX_POINT ( 'NONE', #24999 ) ;
#15568 = ORIENTED_EDGE ( 'NONE', *, *, #9060, .F. ) ;
#15569 = ORIENTED_EDGE ( 'NONE', *, *, #22944, .F. ) ;
#15570 = EDGE_CURVE ( 'NONE', #24947, #18727, #11012, .T. ) ;
#15571 = ORIENTED_EDGE ( 'NONE', *, *, #18920, .F. ) ;
#15572 = DIRECTION ( 'NONE',  ( 0.000000000000000000, 0.000000000000000000, 1.000000000000000000 ) ) ;
#15573 = CARTESIAN_POINT ( 'NONE',  ( -4.000000000000003553, -28.13124999877096855, 6.690598923241489970 ) ) ;
#15574 = CARTESIAN_POINT ( 'NONE',  ( -23.64116323484217830, 20.20656826142297646, 1.000000000000000000 ) ) ;
#15575 = CARTESIAN_POINT ( 'NONE',  ( 23.85222316637486628, 18.19536891688240487, 9.470295877454905309 ) ) ;
#15576 = VECTOR ( 'NONE', #16613, 1000.000000000000000 ) ;
#15577 = CARTESIAN_POINT ( 'NONE',  ( -1.878215178124995832, -5.746835883940462963, 3.440624999385483829 ) ) ;
#15578 = CARTESIAN_POINT ( 'NONE',  ( 4.000000000000003553, -8.999999999999992895, 1.293749998770969079 ) ) ;
#15579 = CARTESIAN_POINT ( 'NONE',  ( -3.369928719974892281E-15, -25.50624999877096855, 4.999999999999992006 ) ) ;
#15580 =( BOUNDED_CURVE ( )  B_SPLINE_CURVE ( 2, ( #22358, #2622, #6533, #18578, #4442, #12415, #14516, #2482, #10450 ),
 .UNSPECIFIED., .F., .F. ) 
 B_SPLINE_CURVE_WITH_KNOTS ( ( 3, 2, 2, 2, 3 ),
 ( 0.5250000000000000222, 0.5333333333333333259, 0.5500000000000000444, 0.5666666666666666519, 0.5750000000000000666 ),
 .UNSPECIFIED. ) 
 CURVE ( )  GEOMETRIC_REPRESENTATION_ITEM ( )  RATIONAL_B_SPLINE_CURVE ( ( 0.9330127018922194093, 0.9330127018922194093, 1.000000000000000000, 0.8660254037844387076, 1.000000000000000000, 0.8660254037844387076, 1.000000000000000000, 0.9330127018922189652, 0.9330127018922194093 ) ) 
 REPRESENTATION_ITEM ( '' )  );
#15581 = CARTESIAN_POINT ( 'NONE',  ( 2.672651547586948120E-15, 27.84062499938548640, 13.33755215474602984 ) ) ;
#15582 = CARTESIAN_POINT ( 'NONE',  ( -3.999999999999996447, -8.999999999999992895, 3.768749998770966947 ) ) ;
#15583 = FACE_OUTER_BOUND ( 'NONE', #22528, .T. ) ;
#15584 = CARTESIAN_POINT ( 'NONE',  ( 2.620986760973688460E-15, -13.61880215351699874, 2.587499999999999467 ) ) ;
#15585 = DIRECTION ( 'NONE',  ( 1.000000000000000000, 0.000000000000000000, 0.000000000000000000 ) ) ;
#15586 = LINE ( 'NONE', #21082, #18725 ) ;
#15587 = CYLINDRICAL_SURFACE ( 'NONE', #19727, 0.5000000000000004441 ) ;
#15588 = CARTESIAN_POINT ( 'NONE',  ( 1.999999999999995781, -27.34374999877097068, 5.535898384862237620 ) ) ;
#15589 = CARTESIAN_POINT ( 'NONE',  ( 3.756430356250002323, 27.01562499938548356, 11.16877607737301226 ) ) ;
#15590 = CARTESIAN_POINT ( 'NONE',  ( 0.000000000000000000, 0.000000000000000000, -6.500000000000000000 ) ) ;
#15591 = CARTESIAN_POINT ( 'NONE',  ( 20.92219106202033529, -23.01025686871653875, -6.500000000000000000 ) ) ;
#15592 = FACE_OUTER_BOUND ( 'NONE', #20705, .T. ) ;
#15593 = ORIENTED_EDGE ( 'NONE', *, *, #3064, .T. ) ;
#15594 = LINE ( 'NONE', #719, #8767 ) ;
#15595 = ORIENTED_EDGE ( 'NONE', *, *, #21632, .F. ) ;
#15596 = VERTEX_POINT ( 'NONE', #12979 ) ;
#15597 = CARTESIAN_POINT ( 'NONE',  ( 0.000000000000000000, 0.000000000000000000, 1.000000000000000000 ) ) ;
#15598 = ORIENTED_EDGE ( 'NONE', *, *, #9244, .F. ) ;
#15599 = CARTESIAN_POINT ( 'NONE',  ( 1.878215178124995832, -28.10312499938548569, 5.746835883940462963 ) ) ;
#15600 = EDGE_CURVE ( 'NONE', #9331, #7533, #3667, .T. ) ;
#15601 = ORIENTED_EDGE ( 'NONE', *, *, #20281, .T. ) ;
#15602 = VERTEX_POINT ( 'NONE', #20818 ) ;
#15603 = LINE ( 'NONE', #5652, #1764 ) ;
#15604 = EDGE_CURVE ( 'NONE', #23080, #9004, #18715, .T. ) ;
#15605 =( GEOMETRIC_REPRESENTATION_CONTEXT ( 3 ) GLOBAL_UNCERTAINTY_ASSIGNED_CONTEXT ( ( #6796 ) ) GLOBAL_UNIT_ASSIGNED_CONTEXT ( ( #9926, #16483, #5884 ) ) REPRESENTATION_CONTEXT ( 'NONE', 'WORKASPACE' ) );
#15606 = ORIENTED_EDGE ( 'NONE', *, *, #21894, .F. ) ;
#15607 = CARTESIAN_POINT ( 'NONE',  ( 4.000000000000003553, 26.35000000000000142, 8.999999999999992895 ) ) ;
#15608 = EDGE_CURVE ( 'NONE', #2274, #13061, #16203, .T. ) ;
#15609 = FACE_OUTER_BOUND ( 'NONE', #8457, .T. ) ;
#15610 = AXIS2_PLACEMENT_3D ( 'NONE', #1088, #19983, #16347 ) ;
#15611 = DIRECTION ( 'NONE',  ( 1.000000000000000000, 0.000000000000000000, 0.000000000000000000 ) ) ;
#15612 = DIRECTION ( 'NONE',  ( 0.000000000000000000, 0.000000000000000000, 1.000000000000000000 ) ) ;
#15613 = CARTESIAN_POINT ( 'NONE',  ( 22.74023967191403628, 17.42784491599521601, 8.999999999999992895 ) ) ;
#15614 = CARTESIAN_POINT ( 'NONE',  ( -3.999999999999999112, 27.45624999877097139, 11.30940107675849404 ) ) ;
#15615 = CARTESIAN_POINT ( 'NONE',  ( 2.000000000000003997, 27.77500000000000213, 5.535898384862238508 ) ) ;
#15616 = CARTESIAN_POINT ( 'NONE',  ( -1.999999999999998224, 29.35000000000000142, 12.46410161513774639 ) ) ;
#15617 = CARTESIAN_POINT ( 'NONE',  ( 21.35910797434536335, 18.70291059638591946, 12.25316411605952283 ) ) ;
#15618 = CARTESIAN_POINT ( 'NONE',  ( -4.000000000000003553, -29.48124999877097352, 6.690598923241489970 ) ) ;
#15619 = STYLED_ITEM ( 'NONE', ( #16057 ), #5978 ) ;
#15620 = ORIENTED_EDGE ( 'NONE', *, *, #11672, .F. ) ;
#15621 = ORIENTED_EDGE ( 'NONE', *, *, #15608, .F. ) ;
#15622 = CARTESIAN_POINT ( 'NONE',  ( -3.756430356249996105, 25.96562499938548996, 11.16877607737301226 ) ) ;
#15623 = AXIS2_PLACEMENT_3D ( 'NONE', #9362, #999, #7000 ) ;
#15624 = VERTEX_POINT ( 'NONE', #8794 ) ;
#15625 = CARTESIAN_POINT ( 'NONE',  ( 13.69242354489141711, 27.92360179968378375, 1.000000000000000000 ) ) ;
#15626 = EDGE_CURVE ( 'NONE', #13988, #7895, #6787, .T. ) ;
#15627 = CARTESIAN_POINT ( 'NONE',  ( 3.756430356250002323, 27.91562499938548569, 11.16877607737301226 ) ) ;
#15628 = CARTESIAN_POINT ( 'NONE',  ( -3.999999999999997335, 27.45624999877096784, 11.30940107675849404 ) ) ;
#15629 = ORIENTED_EDGE ( 'NONE', *, *, #14968, .T. ) ;
#15630 = ORIENTED_EDGE ( 'NONE', *, *, #144, .T. ) ;
#15631 = EDGE_CURVE ( 'NONE', #2787, #6210, #13115, .T. ) ;
#15632 = CARTESIAN_POINT ( 'NONE',  ( 4.000000000000003553, -8.999999999999992895, 4.049999999999998046 ) ) ;
#15633 = ORIENTED_EDGE ( 'NONE', *, *, #24924, .T. ) ;
#15634 = CARTESIAN_POINT ( 'NONE',  ( 0.000000000000000000, 0.000000000000000000, -6.500000000000000000 ) ) ;
#15635 = LINE ( 'NONE', #3852, #5531 ) ;
#15636 = CARTESIAN_POINT ( 'NONE',  ( -1.878215178124996498, 27.54062499938548569, 5.746835883940462963 ) ) ;
#15637 = ORIENTED_EDGE ( 'NONE', *, *, #2589, .T. ) ;
#15638 = CARTESIAN_POINT ( 'NONE',  ( -1.071796769724492338, -26.70759618943233704, 12.99999999999999467 ) ) ;
#15639 = CARTESIAN_POINT ( 'NONE',  ( 4.000000000000001776, 27.70000000000000639, 8.999999999999992895 ) ) ;
#15640 = EDGE_CURVE ( 'NONE', #18698, #4270, #21141, .T. ) ;
#15641 = CARTESIAN_POINT ( 'NONE',  ( 2.672651547586948120E-15, 26.82812499938548356, 13.33755215474602984 ) ) ;
#15642 = CARTESIAN_POINT ( 'NONE',  ( 3.897863563849651936, -30.85476721088028640, 1.000000000000000000 ) ) ;
#15643 = CARTESIAN_POINT ( 'NONE',  ( 1.878215178125004048, 29.26562499938548356, 5.746835883940462963 ) ) ;
#15644 = CARTESIAN_POINT ( 'NONE',  ( -4.648177544792955347E-16, 26.85624999877096997, 4.999999999999991118 ) ) ;
#15645 = CARTESIAN_POINT ( 'NONE',  ( 19.03001124868300309, 19.03001124868292848, 4.381197846482986158 ) ) ;
#15646 = CARTESIAN_POINT ( 'NONE',  ( 18.86200962215296784, 21.51820700011226606, 5.746835883940462963 ) ) ;
#15647 = CARTESIAN_POINT ( 'NONE',  ( 19.14933551713917126, 19.14933551713910376, 12.99999999999999289 ) ) ;
#15648 =( BOUNDED_CURVE ( )  B_SPLINE_CURVE ( 2, ( #473, #6207, #14197, #16430, #5961, #7916, #8058, #6344, #24121 ),
 .UNSPECIFIED., .F., .F. ) 
 B_SPLINE_CURVE_WITH_KNOTS ( ( 3, 2, 2, 2, 3 ),
 ( 0.02500000000000000139, 0.03333333333333333287, 0.05000000000000000278, 0.06666666666666666574, 0.07500000000000001110 ),
 .UNSPECIFIED. ) 
 CURVE ( )  GEOMETRIC_REPRESENTATION_ITEM ( )  RATIONAL_B_SPLINE_CURVE ( ( 0.9330127018922194093, 0.9330127018922194093, 1.000000000000000000, 0.8660254037844387076, 1.000000000000000000, 0.8660254037844387076, 1.000000000000000000, 0.9330127018922191873, 0.9330127018922192983 ) ) 
 REPRESENTATION_ITEM ( '' )  );
#15649 = DIRECTION ( 'NONE',  ( 0.000000000000000000, 0.000000000000000000, 1.000000000000000000 ) ) ;
#15650 = CARTESIAN_POINT ( 'NONE',  ( 0.000000000000000000, 0.000000000000000000, -6.500000000000000000 ) ) ;
#15651 = AXIS2_PLACEMENT_3D ( 'NONE', #22584, #10929, #14601 ) ;
#15652 = CARTESIAN_POINT ( 'NONE',  ( 17.85210898470722896, 23.16450374062589646, 11.16877607737301048 ) ) ;
#15653 = CARTESIAN_POINT ( 'NONE',  ( 5.577813053751546416E-15, 25.95624999877097139, 4.999999999999992006 ) ) ;
#15654 = ORIENTED_EDGE ( 'NONE', *, *, #1933, .F. ) ;
#15655 = CARTESIAN_POINT ( 'NONE',  ( 4.000000000000003553, 26.74374999877096926, 8.999999999999992895 ) ) ;
#15656 = CARTESIAN_POINT ( 'NONE',  ( -4.000000000000001776, -25.86250000000000071, 11.30940107675849760 ) ) ;
#15658 = ORIENTED_EDGE ( 'NONE', *, *, #24165, .T. ) ;
#15657 = DIRECTION ( 'NONE',  ( -0.000000000000000000, -0.000000000000000000, 1.000000000000000000 ) ) ;
#15659 = CARTESIAN_POINT ( 'NONE',  ( -3.756430356249997438, 27.76562499938549067, 11.16877607737301048 ) ) ;
#15660 = LINE ( 'NONE', #25455, #12594 ) ;
#15661 = CARTESIAN_POINT ( 'NONE',  ( 19.58805710660146815, 17.18149551509899453, 20.00001200000000168 ) ) ;
#15662 = CYLINDRICAL_SURFACE ( 'NONE', #22162, 31.10000000000000142 ) ;
#15663 = ORIENTED_EDGE ( 'NONE', *, *, #17656, .T. ) ;
#15664 = ORIENTED_EDGE ( 'NONE', *, *, #3374, .F. ) ;
#15665 = LINE ( 'NONE', #23632, #4705 ) ;
#15666 = CARTESIAN_POINT ( 'NONE',  ( 3.756430356250004987, 29.75312499938549138, 8.999999999999992895 ) ) ;
#15667 = EDGE_CURVE ( 'NONE', #20602, #9588, #9314, .T. ) ;
#15668 = CARTESIAN_POINT ( 'NONE',  ( -3.756430356249997438, -11.16877607737301048, 2.203124999385479565 ) ) ;
#15669 = CARTESIAN_POINT ( 'NONE',  ( 5.577813053751546416E-15, 28.20624999877096784, 4.999999999999992006 ) ) ;
#15670 = CARTESIAN_POINT ( 'NONE',  ( -4.000000000000001776, -27.21250000000000213, 11.30940107675849760 ) ) ;
#15671 = CARTESIAN_POINT ( 'NONE',  ( 2.000000000000005329, 28.67500000000000426, 5.535898384862238508 ) ) ;
#15672 = CARTESIAN_POINT ( 'NONE',  ( 2.000000000000007105, 29.51874999877097139, 5.535898384862238508 ) ) ;
#15673 = CARTESIAN_POINT ( 'NONE',  ( -2.205873879792267900, -29.91968208057595646, 12.34935938736416894 ) ) ;
#15674 = DIRECTION ( 'NONE',  ( 0.000000000000000000, 0.000000000000000000, 1.000000000000000000 ) ) ;
#15675 = CARTESIAN_POINT ( 'NONE',  ( 23.85222316637486273, 18.19536891688240843, 8.999999999999992895 ) ) ;
#15676 = CARTESIAN_POINT ( 'NONE',  ( 16.24135887950949808, 21.89821312900181027, 8.999999999999992895 ) ) ;
#15677 = EDGE_LOOP ( 'NONE', ( #22101, #1535, #23739, #18528 ) ) ;
#15678 = DIRECTION ( 'NONE',  ( -0.000000000000000000, -0.000000000000000000, 1.000000000000000000 ) ) ;
#15679 = CARTESIAN_POINT ( 'NONE',  ( 1.878215178124998497, -28.70312499938548356, 12.25316411605951927 ) ) ;
#15680 = CARTESIAN_POINT ( 'NONE',  ( 3.756430356250003655, 28.40312499938548640, 8.999999999999992895 ) ) ;
#15681 = CARTESIAN_POINT ( 'NONE',  ( 19.78131220369370169, 16.95288507894744257, 5.535898384862238508 ) ) ;
#15682 = CARTESIAN_POINT ( 'NONE',  ( 0.000000000000000000, 0.000000000000000000, 1.000000000000000000 ) ) ;
#15683 = CARTESIAN_POINT ( 'NONE',  ( 3.052426026682831139, 38.91217497027906802, 13.68084836822773553 ) ) ;
#15684 = ORIENTED_EDGE ( 'NONE', *, *, #11818, .T. ) ;
#15685 = DIRECTION ( 'NONE',  ( 1.000000000000000000, 0.000000000000000000, 0.000000000000000000 ) ) ;
#15686 = CARTESIAN_POINT ( 'NONE',  ( 0.000000000000000000, 0.000000000000000000, -6.500000000000000000 ) ) ;
#15688 = ORIENTED_EDGE ( 'NONE', *, *, #17010, .F. ) ;
#15687 = CARTESIAN_POINT ( 'NONE',  ( -23.96296185032722548, -19.82388608118403539, -6.500000000000000000 ) ) ;
#15689 = VERTEX_POINT ( 'NONE', #15323 ) ;
#15690 = CIRCLE ( 'NONE', #4397, 26.00000000000000711 ) ;
#15691 = ORIENTED_EDGE ( 'NONE', *, *, #7872, .T. ) ;
#15692 = ORIENTED_EDGE ( 'NONE', *, *, #15924, .T. ) ;
#15693 = ORIENTED_EDGE ( 'NONE', *, *, #15492, .F. ) ;
#15694 = DIRECTION ( 'NONE',  ( 0.000000000000000000, -0.000000000000000000, 1.000000000000000000 ) ) ;
#15695 = FACE_OUTER_BOUND ( 'NONE', #3052, .T. ) ;
#15696 = EDGE_CURVE ( 'NONE', #10041, #12524, #21339, .T. ) ;
#15697 = CARTESIAN_POINT ( 'NONE',  ( -1.859271017917182139E-15, -29.38749999999999929, 12.99999999999999289 ) ) ;
#15698 = DIRECTION ( 'NONE',  ( 0.6845471059286972748, 0.7289686274214034478, 0.000000000000000000 ) ) ;
#15699 = EDGE_CURVE ( 'NONE', #10594, #6260, #24977, .T. ) ;
#15700 = AXIS2_PLACEMENT_3D ( 'NONE', #24104, #22282, #6187 ) ;
#15701 = CARTESIAN_POINT ( 'NONE',  ( 1.878215178125000939, -12.25316411605952283, 2.315624999385482941 ) ) ;
#15702 = CARTESIAN_POINT ( 'NONE',  ( -3.999999999999996003, -6.690598923241487306, 4.631249998770964993 ) ) ;
#15703 = DIRECTION ( 'NONE',  ( 0.000000000000000000, 0.000000000000000000, 1.000000000000000000 ) ) ;
#15704 = EDGE_CURVE ( 'NONE', #20366, #18357, #19125, .T. ) ;
#15705 = CARTESIAN_POINT ( 'NONE',  ( 1.878215178125000939, 28.32812499938548711, 12.25316411605952283 ) ) ;
#15706 = DIRECTION ( 'NONE',  ( -0.06279051952930156388, 0.9980267284282724471, 0.000000000000000000 ) ) ;
#15707 = CARTESIAN_POINT ( 'NONE',  ( 23.64116323484224225, -20.20656826142291251, -2.750000000000000000 ) ) ;
#15708 = CARTESIAN_POINT ( 'NONE',  ( 2.620986760973688460E-15, -13.61880215351699874, 1.237499999999996270 ) ) ;
#15709 = DIRECTION ( 'NONE',  ( 0.000000000000000000, 0.000000000000000000, 1.000000000000000000 ) ) ;
#15711 = EDGE_CURVE ( 'NONE', #19766, #3578, #23713, .T. ) ;
#15710 = CARTESIAN_POINT ( 'NONE',  ( 4.000000000000003553, 26.29374999877097352, 8.999999999999992895 ) ) ;
#15712 = DIRECTION ( 'NONE',  ( 0.000000000000000000, 1.000000000000000000, 0.000000000000000000 ) ) ;
#15713 = CARTESIAN_POINT ( 'NONE',  ( -4.000000000000001776, -27.15624999877097423, 11.30940107675849760 ) ) ;
#15714 = CARTESIAN_POINT ( 'NONE',  ( -3.756430356249997882, 27.31562499938548427, 11.16877607737301226 ) ) ;
#15715 = CARTESIAN_POINT ( 'NONE',  ( 0.000000000000000000, 0.000000000000000000, -6.500000000000000000 ) ) ;
#15716 = CARTESIAN_POINT ( 'NONE',  ( 15.41874213889396117, -27.00874656207311020, -6.500000000000000000 ) ) ;
#15717 = DIRECTION ( 'NONE',  ( -0.000000000000000000, -1.000000000000000000, -0.000000000000000000 ) ) ;
#15718 = ORIENTED_EDGE ( 'NONE', *, *, #23851, .T. ) ;
#15719 = DIRECTION ( 'NONE',  ( -0.000000000000000000, 0.000000000000000000, 1.000000000000000000 ) ) ;
#15720 = ORIENTED_EDGE ( 'NONE', *, *, #21818, .T. ) ;
#15721 = ORIENTED_EDGE ( 'NONE', *, *, #9329, .F. ) ;
#15722 = CARTESIAN_POINT ( 'NONE',  ( 0.000000000000000000, 10.00000000000000000, 15.00000000000000178 ) ) ;
#15723 = ORIENTED_EDGE ( 'NONE', *, *, #10240, .T. ) ;
#15724 = CARTESIAN_POINT ( 'NONE',  ( 3.756430356249995661, -27.69062499938548427, 6.831223922626973533 ) ) ;
#15725 = ORIENTED_EDGE ( 'NONE', *, *, #25543, .T. ) ;
#15726 = CARTESIAN_POINT ( 'NONE',  ( 1.952785157361432100, -31.03863125411925949, -6.500000000000000000 ) ) ;
#15727 = ORIENTED_EDGE ( 'NONE', *, *, #17721, .T. ) ;
#15728 = CARTESIAN_POINT ( 'NONE',  ( -3.999999999999996003, 27.88750000000000284, 6.690598923241487306 ) ) ;
#15729 = DIRECTION ( 'NONE',  ( 0.000000000000000000, 0.000000000000000000, 1.000000000000000000 ) ) ;
#15730 = EDGE_CURVE ( 'NONE', #25775, #13483, #2013, .T. ) ;
#15731 = CARTESIAN_POINT ( 'NONE',  ( -1.878215178124998497, -12.25316411605951927, 0.5531249993854860936 ) ) ;
#15732 = PRODUCT_RELATED_PRODUCT_CATEGORY ( 'part', '', ( #18425 ) ) ;
#15733 = LINE ( 'NONE', #23189, #9993 ) ;
#15734 = CARTESIAN_POINT ( 'NONE',  ( 15.28000806814115720, 20.59240282405983535, 8.999999999999992895 ) ) ;
#15735 = CARTESIAN_POINT ( 'NONE',  ( 3.469446951953614189E-15, 46.00000000000000000, 8.999999999999992895 ) ) ;
#15736 = PLANE ( 'NONE',  #5453 ) ;
#15737 = ADVANCED_FACE ( 'NONE', ( #21855 ), #23943, .F. ) ;
#15738 = CARTESIAN_POINT ( 'NONE',  ( 4.000000000000003553, 28.15000000000000213, 8.999999999999992895 ) ) ;
#15739 = EDGE_CURVE ( 'NONE', #9082, #4731, #17418, .T. ) ;
#15740 = DIRECTION ( 'NONE',  ( -1.000000000000000000, 0.000000000000000000, 0.000000000000000000 ) ) ;
#15741 = DIRECTION ( 'NONE',  ( 0.000000000000000000, 0.000000000000000000, 1.000000000000000000 ) ) ;
#15742 = ORIENTED_EDGE ( 'NONE', *, *, #13602, .F. ) ;
#15743 = EDGE_LOOP ( 'NONE', ( #5763, #7923, #10813, #13655 ) ) ;
#15744 = CARTESIAN_POINT ( 'NONE',  ( 4.000000000000005329, 29.44374999877097210, 8.999999999999992895 ) ) ;
#15745 = ORIENTED_EDGE ( 'NONE', *, *, #25866, .F. ) ;
#15746 = CARTESIAN_POINT ( 'NONE',  ( -11.91206721063072393, -28.72825533807120735, -6.500000000000000000 ) ) ;
#15747 = CARTESIAN_POINT ( 'NONE',  ( 17.74085449832164585, 19.25660402617361910, 12.99999999999999467 ) ) ;
#15748 = CARTESIAN_POINT ( 'NONE',  ( -11.91206721063010754, 28.72825533807145959, 1.000000000000000000 ) ) ;
#15749 = ORIENTED_EDGE ( 'NONE', *, *, #14683, .T. ) ;
#15750 = VERTEX_POINT ( 'NONE', #23678 ) ;
#15751 = FACE_OUTER_BOUND ( 'NONE', #10713, .T. ) ;
#15752 = ORIENTED_EDGE ( 'NONE', *, *, #15640, .T. ) ;
#15753 = CYLINDRICAL_SURFACE ( 'NONE', #3465, 0.5000000000000004441 ) ;
#15754 = CARTESIAN_POINT ( 'NONE',  ( 2.672651547586948120E-15, 25.47812499938548569, 13.33755215474602984 ) ) ;
#15755 = CARTESIAN_POINT ( 'NONE',  ( -1.878215178124999829, 27.69062499938549138, 12.25316411605951927 ) ) ;
#15756 = CARTESIAN_POINT ( 'NONE',  ( -21.28941499438242246, -22.67092431280570963, -6.500000000000000000 ) ) ;
#15757 = CARTESIAN_POINT ( 'NONE',  ( 4.000000000000005329, 27.25000000000000355, 8.999999999999992895 ) ) ;
#15758 = EDGE_CURVE ( 'NONE', #24490, #10388, #22889, .T. ) ;
#15759 = CARTESIAN_POINT ( 'NONE',  ( -3.756430356249997882, 25.85312499938548925, 11.16877607737301226 ) ) ;
#15760 = FACE_OUTER_BOUND ( 'NONE', #11759, .T. ) ;
#15761 = EDGE_CURVE ( 'NONE', #13301, #8478, #12023, .T. ) ;
#15762 = CARTESIAN_POINT ( 'NONE',  ( 0.000000000000000000, 0.000000000000000000, 20.00001200000000168 ) ) ;
#15763 = CARTESIAN_POINT ( 'NONE',  ( -3.469446951953614189E-15, -30.00000000000000355, 4.999999999999992006 ) ) ;
#15764 = CARTESIAN_POINT ( 'NONE',  ( 16.89101323559370016, 22.54786748508600880, 6.690598923241487306 ) ) ;
#15765 = CARTESIAN_POINT ( 'NONE',  ( 18.22334004483017011, 23.53573480074883761, 8.999999999999992895 ) ) ;
#15766 = CARTESIAN_POINT ( 'NONE',  ( 24.86329371854761661, -18.68225429291740625, -6.500000000000000000 ) ) ;
#15767 = CARTESIAN_POINT ( 'NONE',  ( 1.878215178125000939, 29.11562499938548498, 12.25316411605952283 ) ) ;
#15768 = CARTESIAN_POINT ( 'NONE',  ( 23.34380806741302905, 18.84377675208414971, 6.562149109989046103 ) ) ;
#15769 = CARTESIAN_POINT ( 'NONE',  ( 27.92360179968367362, -13.69242354489162850, -6.500000000000000000 ) ) ;
#15770 = ORIENTED_EDGE ( 'NONE', *, *, #17524, .T. ) ;
#15771 = CARTESIAN_POINT ( 'NONE',  ( 4.000000000000003553, 28.54374999877096997, 8.999999999999992895 ) ) ;
#15772 = CARTESIAN_POINT ( 'NONE',  ( 3.999999999999996447, -25.67500000000000071, 8.999999999999992895 ) ) ;
#15774 = ORIENTED_EDGE ( 'NONE', *, *, #10685, .T. ) ;
#15773 = DIRECTION ( 'NONE',  ( 0.000000000000000000, 1.000000000000000000, 0.000000000000000000 ) ) ;
#15775 = CARTESIAN_POINT ( 'NONE',  ( 1.878215178125004048, 29.37812499938548783, 5.746835883940462963 ) ) ;
#15776 = CARTESIAN_POINT ( 'NONE',  ( -4.393401135981204852, -30.78811501957142127, 1.000000000000000000 ) ) ;
#15777 = CARTESIAN_POINT ( 'NONE',  ( 0.000000000000000000, 0.000000000000000000, -6.500000000000000000 ) ) ;
#15778 = DIRECTION ( 'NONE',  ( 0.5358267949789962126, -0.8443279255020154084, 0.000000000000000000 ) ) ;
#15779 = ORIENTED_EDGE ( 'NONE', *, *, #12435, .T. ) ;
#15780 = ORIENTED_EDGE ( 'NONE', *, *, #2766, .F. ) ;
#15781 = CARTESIAN_POINT ( 'NONE',  ( 3.469446951953614189E-15, 35.50000000000000711, 8.999999999999992895 ) ) ;
#15782 = CARTESIAN_POINT ( 'NONE',  ( 3.756430356250000546, 29.26562499938549067, 11.16877607737301226 ) ) ;
#15783 = CARTESIAN_POINT ( 'NONE',  ( -3.756430356249997438, -11.16877607737301048, 3.103124999385483029 ) ) ;
#15784 =( BOUNDED_CURVE ( )  B_SPLINE_CURVE ( 2, ( #3202, #11308, #10780, #11051, #24921, #6745, #16688, #18774, #14735, #13028, #23213, #19032, #24659, #23098, #16831, #21008, #1114, #25048, #7137, #21249, #15125, #10920, #13158, #11170, #5046, #2956, #4793, #8979, #5297, #17217, #13277, #6999, #1244, #14983, #9228, #25187, #3330, #22712, #12768, #20739, #2817, #864, #8844, #24795, #6877, #4909, #3712, #5807, #25426, #5946, #15507, #7387, #25693, #17456, #19801, #19287, #21899, #25567, #17723, #13415, #13793, #11443, #15365, #3982, #15636, #25815, #23603, #9478, #15755, #1386, #3590, #1507, #1901, #19670, #1776, #9361, #19530, #11694, #17344, #5562, #7650, #3470, #15888, #21510, #3853, #7513, #9864, #9743, #23474, #13545, #13931, #7776, #25309, #11562, #21631, #23860, #1631, #9606, #21769, #23337, #17591, #5427, #5681, #21390, #23718, #13660, #11831, #19414, #17847, #7898, #2402, #8558, #23988, #8169, #10239, #69, #6071, #16274, #10124, #4100, #16148 ),
 .UNSPECIFIED., .F., .T. ) 
 B_SPLINE_CURVE_WITH_KNOTS ( ( 3, 2, 2, 2, 2, 2, 2, 2, 2, 2, 2, 2, 2, 2, 2, 2, 2, 2, 2, 2, 2, 2, 2, 2, 2, 2, 2, 2, 2, 2, 2, 2, 2, 2, 2, 2, 2, 2, 2, 2, 2, 2, 2, 2, 2, 2, 2, 2, 2, 2, 2, 2, 2, 2, 2, 2, 2, 2, 2, 2, 3 ),
 ( 0.000000000000000000, 0.01666666666666666644, 0.03333333333333333287, 0.05000000000000000278, 0.06666666666666666574, 0.08333333333333332871, 0.1000000000000000056, 0.1166666666666666685, 0.1333333333333333315, 0.1499999999999999944, 0.1666666666666666574, 0.1833333333333333204, 0.2000000000000000111, 0.2166666666666666741, 0.2333333333333333370, 0.2500000000000000000, 0.2666666666666666630, 0.2833333333333333259, 0.2999999999999999889, 0.3166666666666666519, 0.3333333333333333148, 0.3499999999999999778, 0.3666666666666666408, 0.3833333333333333592, 0.4000000000000000222, 0.4166666666666666852, 0.4333333333333333481, 0.4500000000000000111, 0.4666666666666666741, 0.4833333333333333370, 0.5000000000000000000, 0.5166666666666667185, 0.5333333333333333259, 0.5500000000000000444, 0.5666666666666666519, 0.5833333333333333703, 0.5999999999999999778, 0.6166666666666666963, 0.6333333333333333037, 0.6500000000000000222, 0.6666666666666666297, 0.6833333333333333481, 0.6999999999999999556, 0.7166666666666666741, 0.7333333333333332815, 0.7500000000000000000, 0.7666666666666667185, 0.7833333333333333259, 0.8000000000000000444, 0.8166666666666666519, 0.8333333333333333703, 0.8499999999999999778, 0.8666666666666666963, 0.8833333333333333037, 0.9000000000000000222, 0.9166666666666666297, 0.9333333333333333481, 0.9499999999999999556, 0.9666666666666666741, 0.9833333333333332815, 1.000000000000000000 ),
 .UNSPECIFIED. ) 
 CURVE ( )  GEOMETRIC_REPRESENTATION_ITEM ( )  RATIONAL_B_SPLINE_CURVE ( ( 1.000000000000000000, 0.8660254037844387076, 1.000000000000000000, 0.8660254037844387076, 1.000000000000000000, 0.8660254037844387076, 1.000000000000000000, 0.8660254037844387076, 1.000000000000000000, 0.8660254037844387076, 1.000000000000000000, 0.8660254037844387076, 1.000000000000000000, 0.8660254037844387076, 1.000000000000000000, 0.8660254037844387076, 1.000000000000000000, 0.8660254037844387076, 1.000000000000000000, 0.8660254037844387076, 1.000000000000000000, 0.8660254037844387076, 1.000000000000000000, 0.8660254037844387076, 1.000000000000000000, 0.8660254037844387076, 1.000000000000000000, 0.8660254037844387076, 1.000000000000000000, 0.8660254037844387076, 1.000000000000000000, 0.8660254037844387076, 1.000000000000000000, 0.8660254037844387076, 1.000000000000000000, 0.8660254037844387076, 1.000000000000000000, 0.8660254037844387076, 1.000000000000000000, 0.8660254037844387076, 1.000000000000000000, 0.8660254037844387076, 1.000000000000000000, 0.8660254037844387076, 1.000000000000000000, 0.8660254037844387076, 1.000000000000000000, 0.8660254037844387076, 1.000000000000000000, 0.8660254037844387076, 1.000000000000000000, 0.8660254037844387076, 1.000000000000000000, 0.8660254037844387076, 1.000000000000000000, 0.8660254037844387076, 1.000000000000000000, 0.8660254037844387076, 1.000000000000000000, 0.8660254037844387076, 1.000000000000000000, 0.8660254037844387076, 1.000000000000000000, 0.8660254037844387076, 1.000000000000000000, 0.8660254037844387076, 1.000000000000000000, 0.8660254037844387076, 1.000000000000000000, 0.8660254037844387076, 1.000000000000000000, 0.8660254037844387076, 1.000000000000000000, 0.8660254037844387076, 1.000000000000000000, 0.8660254037844387076, 1.000000000000000000, 0.8660254037844387076, 1.000000000000000000, 0.8660254037844387076, 1.000000000000000000, 0.8660254037844387076, 1.000000000000000000, 0.8660254037844387076, 1.000000000000000000, 0.8660254037844387076, 1.000000000000000000, 0.8660254037844387076, 1.000000000000000000, 0.8660254037844387076, 1.000000000000000000, 0.8660254037844387076, 1.000000000000000000, 0.8660254037844387076, 1.000000000000000000, 0.8660254037844387076, 1.000000000000000000, 0.8660254037844387076, 1.000000000000000000, 0.8660254037844387076, 1.000000000000000000, 0.8660254037844387076, 1.000000000000000000, 0.8660254037844387076, 1.000000000000000000, 0.8660254037844387076, 1.000000000000000000, 0.8660254037844387076, 1.000000000000000000, 0.8660254037844387076, 1.000000000000000000, 0.8660254037844387076, 1.000000000000000000, 0.8660254037844387076, 1.000000000000000000, 0.8660254037844387076, 1.000000000000000000, 0.8660254037844387076, 1.000000000000000000, 0.8660254037844387076, 1.000000000000000000 ) ) 
 REPRESENTATION_ITEM ( '' )  );
#15785 = CARTESIAN_POINT ( 'NONE',  ( -3.999999999999996447, 28.28124999877097778, 6.690598923241487306 ) ) ;
#15786 = FILL_AREA_STYLE_COLOUR ( '', #18551 ) ;
#15787 = EDGE_CURVE ( 'NONE', #19787, #8351, #7850, .T. ) ;
#15788 = LINE ( 'NONE', #5848, #20987 ) ;
#15789 =( BOUNDED_CURVE ( )  B_SPLINE_CURVE ( 2, ( #8858, #12903, #16456, #8592, #4527, #18543, #22974, #2967, #16845 ),
 .UNSPECIFIED., .F., .F. ) 
 B_SPLINE_CURVE_WITH_KNOTS ( ( 3, 2, 2, 2, 3 ),
 ( 0.07500000000000001110, 0.08333333333333332871, 0.1000000000000000056, 0.1166666666666666685, 0.1250000000000000000 ),
 .UNSPECIFIED. ) 
 CURVE ( )  GEOMETRIC_REPRESENTATION_ITEM ( )  RATIONAL_B_SPLINE_CURVE ( ( 0.9330127018922192983, 0.9330127018922194093, 1.000000000000000000, 0.8660254037844387076, 1.000000000000000000, 0.8660254037844387076, 1.000000000000000000, 0.9330127018922194093, 0.9330127018922194093 ) ) 
 REPRESENTATION_ITEM ( '' )  );
#15790 = DIRECTION ( 'NONE',  ( 1.000000000000000000, 0.000000000000000000, 0.000000000000000000 ) ) ;
#15791 = DIRECTION ( 'NONE',  ( -0.000000000000000000, -0.000000000000000000, 1.000000000000000000 ) ) ;
#15792 = AXIS2_PLACEMENT_3D ( 'NONE', #9310, #17028, #21582 ) ;
#15793 = CARTESIAN_POINT ( 'NONE',  ( -1.152368580279349075, -29.97923206407486774, 12.84165680230635509 ) ) ;
#15794 = CARTESIAN_POINT ( 'NONE',  ( 21.21320343559646915, 21.21320343559638744, 12.99999999999999289 ) ) ;
#15795 = LINE ( 'NONE', #16064, #14565 ) ;
#15796 = CARTESIAN_POINT ( 'NONE',  ( 15.26024822061316399, 20.91710247010547619, 6.690598923241487306 ) ) ;
#15797 = EDGE_LOOP ( 'NONE', ( #1204, #13898, #13258, #17009 ) ) ;
#15798 = CARTESIAN_POINT ( 'NONE',  ( -5.254586613389494509, 39.00010698140259535, 10.62610181236646056 ) ) ;
#15799 = DIRECTION ( 'NONE',  ( -0.000000000000000000, -1.000000000000000000, -0.000000000000000000 ) ) ;
#15800 = CARTESIAN_POINT ( 'NONE',  ( 1.878215178125000939, 27.87812499938548427, 12.25316411605952283 ) ) ;
#15801 = EDGE_CURVE ( 'NONE', #13892, #14800, #7730, .T. ) ;
#15802 = CARTESIAN_POINT ( 'NONE',  ( 2.000000000000003997, -5.535898384862238508, 2.325000000000000622 ) ) ;
#15803 = CARTESIAN_POINT ( 'NONE',  ( -31.09598070739550124, 0.4999838450261748779, 1.000000000000000000 ) ) ;
#15804 = CARTESIAN_POINT ( 'NONE',  ( 3.170271286762905927, 39.00010698140257404, 13.49491574449624665 ) ) ;
#15805 = ORIENTED_EDGE ( 'NONE', *, *, #23366, .F. ) ;
#15806 = CARTESIAN_POINT ( 'NONE',  ( 3.756430356250000546, 29.26562499938549067, 11.16877607737301226 ) ) ;
#15807 = DIRECTION ( 'NONE',  ( 0.9980267284282724471, 0.06279051952930156388, 0.000000000000000000 ) ) ;
#15809 = ORIENTED_EDGE ( 'NONE', *, *, #18852, .T. ) ;
#15808 = FACE_OUTER_BOUND ( 'NONE', #19015, .T. ) ;
#15810 = ADVANCED_FACE ( 'NONE', ( #9556, #5755 ), #3805, .F. ) ;
#15811 = VERTEX_POINT ( 'NONE', #11785 ) ;
#15812 = CIRCLE ( 'NONE', #7031, 31.10000000000000142 ) ;
#15813 = ORIENTED_EDGE ( 'NONE', *, *, #7588, .F. ) ;
#15814 = ORIENTED_EDGE ( 'NONE', *, *, #239, .T. ) ;
#15815 = AXIS2_PLACEMENT_3D ( 'NONE', #11319, #19299, #19540 ) ;
#15816 = VERTEX_POINT ( 'NONE', #1857 ) ;
#15817 = CARTESIAN_POINT ( 'NONE',  ( 0.7500000000000001110, 20.00000000000000000, 17.69999999999999929 ) ) ;
#15818 = LINE ( 'NONE', #19600, #20715 ) ;
#15819 = FILL_AREA_STYLE_COLOUR ( '', #5571 ) ;
#15820 = CARTESIAN_POINT ( 'NONE',  ( -3.756430356249994773, 25.81562499938548783, 8.999999999999992895 ) ) ;
#15821 = CARTESIAN_POINT ( 'NONE',  ( 3.756430356250002323, -11.16877607737301226, 3.703124999385482674 ) ) ;
#15822 = CARTESIAN_POINT ( 'NONE',  ( -3.999999999999996447, -8.999999999999992895, 3.768749998770966947 ) ) ;
#15823 = DIRECTION ( 'NONE',  ( 1.000000000000000000, 0.000000000000000000, 0.000000000000000000 ) ) ;
#15824 = CARTESIAN_POINT ( 'NONE',  ( 1.878215178125004048, 29.37812499938548783, 5.746835883940462963 ) ) ;
#15825 = CARTESIAN_POINT ( 'NONE',  ( 29.41953157733093960, 10.08469938919488484, 1.000000000000000000 ) ) ;
#15826 = CARTESIAN_POINT ( 'NONE',  ( 3.878215178125003604, 29.57031249969274356, 8.999999999999992895 ) ) ;
#15827 = CARTESIAN_POINT ( 'NONE',  ( 2.000000000000000888, -12.46410161513774817, 0.8249999999999992895 ) ) ;
#15828 = CIRCLE ( 'NONE', #22033, 31.10000000000000142 ) ;
#15829 = DIRECTION ( 'NONE',  ( 0.000000000000000000, -1.000000000000000000, 0.000000000000000000 ) ) ;
#15830 = CARTESIAN_POINT ( 'NONE',  ( 5.577813053751546416E-15, 25.73124999877097352, 12.99999999999999289 ) ) ;
#15831 = CARTESIAN_POINT ( 'NONE',  ( 4.000000000000001776, 27.70000000000000639, 8.999999999999992895 ) ) ;
#15832 = CARTESIAN_POINT ( 'NONE',  ( -4.000000000000003553, -29.03124999877096712, 6.690598923241489970 ) ) ;
#15833 = CARTESIAN_POINT ( 'NONE',  ( 3.735045420075836212E-15, 27.61562499938548498, 4.662447845253954171 ) ) ;
#15834 = DIRECTION ( 'NONE',  ( -0.9685831611286283005, 0.2486898871648657861, 0.000000000000000000 ) ) ;
#15835 = ADVANCED_FACE ( 'NONE', ( #9818 ), #1465, .F. ) ;
#15837 = CARTESIAN_POINT ( 'NONE',  ( 21.21320343559646915, 21.21320343559638744, 8.999999999999992895 ) ) ;
#15836 = VECTOR ( 'NONE', #6626, 1000.000000000000000 ) ;
#15838 = CARTESIAN_POINT ( 'NONE',  ( 28.14012133169324414, 13.24173596767369254, -6.500000000000000000 ) ) ;
#15839 = ORIENTED_EDGE ( 'NONE', *, *, #16128, .F. ) ;
#15840 = DIRECTION ( 'NONE',  ( 0.000000000000000000, -0.000000000000000000, 1.000000000000000000 ) ) ;
#15841 = VERTEX_POINT ( 'NONE', #25520 ) ;
#15842 = EDGE_CURVE ( 'NONE', #6572, #17588, #12441, .T. ) ;
#15843 = ORIENTED_EDGE ( 'NONE', *, *, #19030, .F. ) ;
#15844 = CARTESIAN_POINT ( 'NONE',  ( 0.000000000000000000, 31.50000000000000000, 14.99999999999999289 ) ) ;
#15845 = ORIENTED_EDGE ( 'NONE', *, *, #9378, .T. ) ;
#15846 = ADVANCED_FACE ( 'NONE', ( #3547 ), #21587, .T. ) ;
#15847 = CARTESIAN_POINT ( 'NONE',  ( -2.672651547586948120E-15, -27.39062499938548356, 13.33755215474602984 ) ) ;
#15848 = ORIENTED_EDGE ( 'NONE', *, *, #2469, .T. ) ;
#15849 = DIRECTION ( 'NONE',  ( -0.000000000000000000, 0.000000000000000000, 1.000000000000000000 ) ) ;
#15850 = AXIS2_PLACEMENT_3D ( 'NONE', #24547, #10419, #6389 ) ;
#15851 = VERTEX_POINT ( 'NONE', #11520 ) ;
#15852 = EDGE_CURVE ( 'NONE', #17935, #18582, #9940, .T. ) ;
#15853 = CARTESIAN_POINT ( 'NONE',  ( -20.20656826142249685, 23.64116323484259752, 1.000000000000000000 ) ) ;
#15854 = CARTESIAN_POINT ( 'NONE',  ( 3.756430356250003211, 26.64062499938548356, 6.831223922626973533 ) ) ;
#15855 = CIRCLE ( 'NONE', #12085, 31.10000000000000142 ) ;
#15856 = AXIS2_PLACEMENT_3D ( 'NONE', #14970, #4898, #17205 ) ;
#15857 = CARTESIAN_POINT ( 'NONE',  ( -0.5000000000000001110, 0.000000000000000000, 16.00000000000000000 ) ) ;
#15858 = DIRECTION ( 'NONE',  ( -0.7071067811865487940, -0.7071067811865463515, 0.000000000000000000 ) ) ;
#15859 = CARTESIAN_POINT ( 'NONE',  ( 19.84539375530421168, 19.84539375530412997, 4.662447845253954171 ) ) ;
#15860 = CARTESIAN_POINT ( 'NONE',  ( 3.469446951953614189E-15, 40.00000000000000000, 8.999999999999992895 ) ) ;
#15861 = CARTESIAN_POINT ( 'NONE',  ( 3.526711513754818395, 31.50000000000000000, 4.645898033750289535 ) ) ;
#15863 = AXIS2_PLACEMENT_3D ( 'NONE', #9147, #13087, #3141 ) ;
#15862 = APPLICATION_PROTOCOL_DEFINITION ( 'draft international standard', 'automotive_design', 1998, #25153 ) ;
#15864 = EDGE_CURVE ( 'NONE', #7056, #7828, #20147, .T. ) ;
#15865 = CARTESIAN_POINT ( 'NONE',  ( -1.999999999999995781, 29.19999999999999929, 5.535898384862237620 ) ) ;
#15866 = CARTESIAN_POINT ( 'NONE',  ( 3.756430356250003655, -8.999999999999992895, 0.2531249993854844949 ) ) ;
#15867 = CARTESIAN_POINT ( 'NONE',  ( 17.58694394176227149, 22.89933869768094610, 8.999999999999992895 ) ) ;
#15868 = DIRECTION ( 'NONE',  ( 0.000000000000000000, -0.000000000000000000, 1.000000000000000000 ) ) ;
#15869 = ORIENTED_EDGE ( 'NONE', *, *, #16767, .T. ) ;
#15870 = VERTEX_POINT ( 'NONE', #18193 ) ;
#15871 = CARTESIAN_POINT ( 'NONE',  ( -1.878215178124998275, 25.55312499938549564, 12.25316411605951927 ) ) ;
#15872 = CIRCLE ( 'NONE', #22117, 6.000000000000000000 ) ;
#15873 = EDGE_CURVE ( 'NONE', #14980, #5929, #6186, .T. ) ;
#15874 = ORIENTED_EDGE ( 'NONE', *, *, #6465, .F. ) ;
#15875 = DIRECTION ( 'NONE',  ( 0.9685831611286337406, 0.2486898871648445808, 0.000000000000000000 ) ) ;
#15876 = CARTESIAN_POINT ( 'NONE',  ( 1.878215178125000939, 25.62812499938548783, 12.25316411605952283 ) ) ;
#15877 = CARTESIAN_POINT ( 'NONE',  ( 1.878215178125000939, 29.22812499938548569, 12.25316411605952283 ) ) ;
#15878 = CARTESIAN_POINT ( 'NONE',  ( 2.000000000000000888, 28.01874999877096784, 12.46410161513774817 ) ) ;
#15879 = VERTEX_POINT ( 'NONE', #10317 ) ;
#15880 = EDGE_CURVE ( 'NONE', #7544, #8072, #22097, .T. ) ;
#15881 = ORIENTED_EDGE ( 'NONE', *, *, #6827, .T. ) ;
#15882 = CARTESIAN_POINT ( 'NONE',  ( 3.999999999999995559, -25.63749999999999929, 6.690598923241487306 ) ) ;
#15883 = AXIS2_PLACEMENT_3D ( 'NONE', #3844, #13922, #7641 ) ;
#15884 = VERTEX_POINT ( 'NONE', #12551 ) ;
#15885 = EDGE_CURVE ( 'NONE', #15986, #20362, #22359, .T. ) ;
#15886 = DIRECTION ( 'NONE',  ( 0.000000000000000000, 1.000000000000000000, 0.000000000000000000 ) ) ;
#15887 = DIRECTION ( 'NONE',  ( 0.000000000000000000, 0.000000000000000000, 1.000000000000000000 ) ) ;
#15888 = CARTESIAN_POINT ( 'NONE',  ( 1.878215178124998275, 28.21562499938549351, 12.25316411605952283 ) ) ;
#15889 = VECTOR ( 'NONE', #1018, 1000.000000000000000 ) ;
#15890 = CARTESIAN_POINT ( 'NONE',  ( -18.28012134629558716, 25.16042852506110705, -6.500000000000000000 ) ) ;
#15891 = CARTESIAN_POINT ( 'NONE',  ( 4.000000000000001776, 29.40624999877096357, 11.30940107675849760 ) ) ;
#15892 = CARTESIAN_POINT ( 'NONE',  ( 0.000000000000000000, 28.03750000000001208, 13.61880215351699874 ) ) ;
#15893 = AXIS2_PLACEMENT_3D ( 'NONE', #7597, #5632, #7722 ) ;
#15894 = FACE_OUTER_BOUND ( 'NONE', #25172, .T. ) ;
#15895 = DIRECTION ( 'NONE',  ( 1.000000000000000000, 0.000000000000000000, 0.000000000000000000 ) ) ;
#15896 = AXIS2_PLACEMENT_3D ( 'NONE', #13644, #3692, #302 ) ;
#15897 = DIRECTION ( 'NONE',  ( 1.000000000000000000, 0.000000000000000000, 0.000000000000000000 ) ) ;
#15898 = CARTESIAN_POINT ( 'NONE',  ( 20.73590635829554429, 17.90747923354928162, 5.535898384862238508 ) ) ;
#15899 = CARTESIAN_POINT ( 'NONE',  ( 16.63234978716043244, 21.94474454307910705, 8.999999999999992895 ) ) ;
#15900 = DIRECTION ( 'NONE',  ( 1.000000000000000000, 0.000000000000000000, -0.000000000000000000 ) ) ;
#15901 = CARTESIAN_POINT ( 'NONE',  ( 1.071796769724487675, 29.53615380933863221, 4.999999999999988454 ) ) ;
#15902 = AXIS2_PLACEMENT_3D ( 'NONE', #16358, #2476, #16216 ) ;
#15903 = DIRECTION ( 'NONE',  ( 1.000000000000000000, 0.000000000000000000, 0.000000000000000000 ) ) ;
#15904 = AXIS2_PLACEMENT_3D ( 'NONE', #24478, #10728, #8145 ) ;
#15905 = CARTESIAN_POINT ( 'NONE',  ( 17.87326343783943017, 25.45105997952919097, -6.500000000000000000 ) ) ;
#15906 = ORIENTED_EDGE ( 'NONE', *, *, #24557, .F. ) ;
#15907 = CARTESIAN_POINT ( 'NONE',  ( -1.999999999999998224, 27.04374999877096641, 12.46410161513774639 ) ) ;
#15908 = CARTESIAN_POINT ( 'NONE',  ( -3.752267015613588906E-15, -26.01249999999999929, 4.381197846482986158 ) ) ;
#15910 = VERTEX_POINT ( 'NONE', #2623 ) ;
#15909 = CARTESIAN_POINT ( 'NONE',  ( 1.878215178125008489, 26.22812499938548925, 5.746835883940462963 ) ) ;
#15911 = CIRCLE ( 'NONE', #21344, 31.10000000000000142 ) ;
#15912 = CARTESIAN_POINT ( 'NONE',  ( 3.756430356250003211, 27.54062499938547859, 6.831223922626973533 ) ) ;
#15913 = CIRCLE ( 'NONE', #18408, 0.5000000000000002220 ) ;
#15914 = PLANE ( 'NONE',  #23888 ) ;
#15915 = DIRECTION ( 'NONE',  ( 0.000000000000000000, 0.000000000000000000, 1.000000000000000000 ) ) ;
#15916 = CARTESIAN_POINT ( 'NONE',  ( 26.25859848311271705, 16.66421332384673804, -6.500000000000000000 ) ) ;
#15917 = ORIENTED_EDGE ( 'NONE', *, *, #11622, .T. ) ;
#15918 = ORIENTED_EDGE ( 'NONE', *, *, #15626, .T. ) ;
#15919 = EDGE_CURVE ( 'NONE', #22563, #10227, #24191, .T. ) ;
#15920 = CARTESIAN_POINT ( 'NONE',  ( -3.756430356249994773, 29.07812499938548711, 8.999999999999992895 ) ) ;
#15921 = EDGE_CURVE ( 'NONE', #13306, #21660, #16241, .T. ) ;
#15922 = CIRCLE ( 'NONE', #20966, 0.4999999999999998890 ) ;
#15923 = CARTESIAN_POINT ( 'NONE',  ( 3.756430356250003655, -8.999999999999992895, 2.390624999385481342 ) ) ;
#15924 = EDGE_CURVE ( 'NONE', #1533, #3918, #352, .T. ) ;
#15925 = AXIS2_PLACEMENT_3D ( 'NONE', #9488, #11455, #21265 ) ;
#15926 = EDGE_CURVE ( 'NONE', #7709, #11678, #19974, .T. ) ;
#15927 = DIRECTION ( 'NONE',  ( -0.000000000000000000, -0.000000000000000000, 1.000000000000000000 ) ) ;
#15928 = DIRECTION ( 'NONE',  ( -0.000000000000000000, -1.000000000000000000, -0.000000000000000000 ) ) ;
#15929 = AXIS2_PLACEMENT_3D ( 'NONE', #11450, #11061, #19421 ) ;
#15930 = DIRECTION ( 'NONE',  ( 0.000000000000000000, 0.000000000000000000, 1.000000000000000000 ) ) ;
#15931 = CARTESIAN_POINT ( 'NONE',  ( 1.071796769724489895, 29.35134618820331198, 12.99999999999999467 ) ) ;
#15932 = CARTESIAN_POINT ( 'NONE',  ( 22.67092431280594056, 21.28941499438218088, -6.500000000000000000 ) ) ;
#15933 = CARTESIAN_POINT ( 'NONE',  ( 20.89942480057588980, 20.89942480057579033, 4.999999999999992006 ) ) ;
#15934 = CARTESIAN_POINT ( 'NONE',  ( -1.999999999999998224, -12.46410161513774639, 2.043749998770966414 ) ) ;
#15935 = CARTESIAN_POINT ( 'NONE',  ( 16.96614333022570875, 19.79457045497182577, 5.535898384862237620 ) ) ;
#15936 = EDGE_LOOP ( 'NONE', ( #19377, #3489, #15187, #14790 ) ) ;
#15937 = DIRECTION ( 'NONE',  ( 1.000000000000000000, 0.000000000000000000, 0.000000000000000000 ) ) ;
#15938 = CARTESIAN_POINT ( 'NONE',  ( 3.013468763610312351, 29.84883905190463338, 6.356741067357151387 ) ) ;
#15939 = CARTESIAN_POINT ( 'NONE',  ( -1.878215178124995832, 26.75312499938548783, 5.746835883940462963 ) ) ;
#15940 = CYLINDRICAL_SURFACE ( 'NONE', #783, 4.000000000000000000 ) ;
#15941 = VECTOR ( 'NONE', #1661, 1000.000000000000000 ) ;
#15942 = CARTESIAN_POINT ( 'NONE',  ( -1.071796769724487230, 26.42634618820330061, 4.999999999999992006 ) ) ;
#15943 = CARTESIAN_POINT ( 'NONE',  ( 3.749140371009410000, 38.71721868403346178, 13.40281365441718542 ) ) ;
#15944 = ORIENTED_EDGE ( 'NONE', *, *, #24471, .T. ) ;
#15945 = DIRECTION ( 'NONE',  ( 0.000000000000000000, 0.000000000000000000, 1.000000000000000000 ) ) ;
#15946 = CARTESIAN_POINT ( 'NONE',  ( -3.999999999999996003, 26.03124999877097068, 6.690598923241487306 ) ) ;
#15947 = DIRECTION ( 'NONE',  ( 0.000000000000000000, 0.000000000000000000, -1.000000000000000000 ) ) ;
#15949 = ORIENTED_EDGE ( 'NONE', *, *, #6190, .F. ) ;
#15948 = CARTESIAN_POINT ( 'NONE',  ( 1.071796769724487230, -26.42634618820330061, 4.999999999999992006 ) ) ;
#15950 = CIRCLE ( 'NONE', #25538, 31.10000000000000142 ) ;
#15951 = AXIS2_PLACEMENT_3D ( 'NONE', #20815, #17415, #19233 ) ;
#15952 = ORIENTED_EDGE ( 'NONE', *, *, #7141, .T. ) ;
#15953 = ORIENTED_EDGE ( 'NONE', *, *, #18568, .T. ) ;
#15954 = EDGE_LOOP ( 'NONE', ( #9178, #22611, #25525, #13634 ) ) ;
#15955 = CARTESIAN_POINT ( 'NONE',  ( 25.99519186311192342, -0.5000000000000000000, 19.50000000000000000 ) ) ;
#15956 =( BOUNDED_CURVE ( )  B_SPLINE_CURVE ( 2, ( #18888, #20586, #6853, #10634, #20981, #18626, #16929, #5018, #13001 ),
 .UNSPECIFIED., .F., .F. ) 
 B_SPLINE_CURVE_WITH_KNOTS ( ( 3, 2, 2, 2, 3 ),
 ( 0.3250000000000000111, 0.3333333333333333148, 0.3499999999999999778, 0.3666666666666666408, 0.3750000000000000000 ),
 .UNSPECIFIED. ) 
 CURVE ( )  GEOMETRIC_REPRESENTATION_ITEM ( )  RATIONAL_B_SPLINE_CURVE ( ( 0.9330127018922194093, 0.9330127018922196314, 1.000000000000000000, 0.8660254037844387076, 1.000000000000000000, 0.8660254037844387076, 1.000000000000000000, 0.9330127018922194093, 0.9330127018922194093 ) ) 
 REPRESENTATION_ITEM ( '' )  );
#15958 = CARTESIAN_POINT ( 'NONE',  ( 30.45149776762729488, 6.317933499823326748, -2.750000000000000000 ) ) ;
#15957 = VECTOR ( 'NONE', #6443, 1000.000000000000000 ) ;
#15959 = EDGE_CURVE ( 'NONE', #24155, #17175, #11442, .T. ) ;
#15960 = CARTESIAN_POINT ( 'NONE',  ( 1.878215178125006934, 26.56562499938548783, 5.746835883940462963 ) ) ;
#15961 =( BOUNDED_CURVE ( )  B_SPLINE_CURVE ( 2, ( #20224, #2320, #4776, #11153, #22940, #20845, #9462, #21228, #1489 ),
 .UNSPECIFIED., .F., .F. ) 
 B_SPLINE_CURVE_WITH_KNOTS ( ( 3, 2, 2, 2, 3 ),
 ( 0.2750000000000000222, 0.2833333333333333259, 0.2999999999999999889, 0.3166666666666666519, 0.3250000000000000111 ),
 .UNSPECIFIED. ) 
 CURVE ( )  GEOMETRIC_REPRESENTATION_ITEM ( )  RATIONAL_B_SPLINE_CURVE ( ( 0.9330127018922194093, 0.9330127018922196314, 1.000000000000000000, 0.8660254037844387076, 1.000000000000000000, 0.8660254037844387076, 1.000000000000000000, 0.9330127018922191873, 0.9330127018922194093 ) ) 
 REPRESENTATION_ITEM ( '' )  );
#15962 = VECTOR ( 'NONE', #14114, 1000.000000000000000 ) ;
#15963 = CARTESIAN_POINT ( 'NONE',  ( 3.756430356250004099, -6.831223922626973533, 3.328124999385480898 ) ) ;
#15964 = CARTESIAN_POINT ( 'NONE',  ( 4.000000000000003553, -8.999999999999992895, 4.893749998770967835 ) ) ;
#15965 = SURFACE_STYLE_USAGE ( .BOTH. , #14260 ) ;
#15966 = AXIS2_PLACEMENT_3D ( 'NONE', #8724, #14756, #11191 ) ;
#15967 = CARTESIAN_POINT ( 'NONE',  ( -1.878215178124998497, 28.25312499938548427, 12.25316411605951927 ) ) ;
#15968 = VECTOR ( 'NONE', #17799, 1000.000000000000000 ) ;
#15969 = EDGE_CURVE ( 'NONE', #3288, #10049, #19538, .T. ) ;
#15970 = CARTESIAN_POINT ( 'NONE',  ( -16.66421332384646448, 26.25859848311288403, -6.500000000000000000 ) ) ;
#15971 = CARTESIAN_POINT ( 'NONE',  ( 4.000000000000003553, -8.999999999999992895, 0.9000000000000014655 ) ) ;
#15972 = CARTESIAN_POINT ( 'NONE',  ( -1.878215178124998497, 25.89062499938548356, 12.25316411605951927 ) ) ;
#15973 = VECTOR ( 'NONE', #15364, 1000.000000000000000 ) ;
#15974 = LINE ( 'NONE', #18441, #21322 ) ;
#15975 = CARTESIAN_POINT ( 'NONE',  ( 4.000000000000000888, 26.25624999877096499, 11.30940107675849760 ) ) ;
#15976 = DIRECTION ( 'NONE',  ( 1.000000000000000000, 0.000000000000000000, 0.000000000000000000 ) ) ;
#15977 = CARTESIAN_POINT ( 'NONE',  ( -4.000000000000001776, -29.85624999877096997, 11.30940107675849760 ) ) ;
#15978 = AXIS2_PLACEMENT_3D ( 'NONE', #24243, #6331, #18504 ) ;
#15979 = CARTESIAN_POINT ( 'NONE',  ( 3.756430356250003655, 27.50312499938548427, 8.999999999999992895 ) ) ;
#15980 = CARTESIAN_POINT ( 'NONE',  ( 0.000000000000000000, 0.000000000000000000, 17.69999999999999929 ) ) ;
#15981 = CYLINDRICAL_SURFACE ( 'NONE', #10819, 31.10000000000000142 ) ;
#15982 = DIRECTION ( 'NONE',  ( 0.7071067811865487940, 0.7071067811865463515, 0.000000000000000000 ) ) ;
#15983 = ORIENTED_EDGE ( 'NONE', *, *, #19707, .T. ) ;
#15984 = DIRECTION ( 'NONE',  ( -0.9048270524660229075, -0.4257792915650654986, 0.000000000000000000 ) ) ;
#15986 = VERTEX_POINT ( 'NONE', #22238 ) ;
#15985 = CARTESIAN_POINT ( 'NONE',  ( 3.756430356249996105, -29.37812499938548427, 6.831223922626973533 ) ) ;
#15987 = AXIS2_PLACEMENT_3D ( 'NONE', #9297, #15435, #25249 ) ;
#15988 = ORIENTED_EDGE ( 'NONE', *, *, #12397, .F. ) ;
#15989 = CARTESIAN_POINT ( 'NONE',  ( 5.577813053751546416E-15, 27.81250000000000355, 4.999999999999992006 ) ) ;
#15990 = ORIENTED_EDGE ( 'NONE', *, *, #3818, .F. ) ;
#15991 = VERTEX_POINT ( 'NONE', #4321 ) ;
#15992 = DIRECTION ( 'NONE',  ( -0.000000000000000000, 0.000000000000000000, 1.000000000000000000 ) ) ;
#15993 = EDGE_LOOP ( 'NONE', ( #4757, #14549, #1028, #15693 ) ) ;
#15994 = CARTESIAN_POINT ( 'NONE',  ( -12.78762572734017411, 28.34936733434218681, -6.500000000000000000 ) ) ;
#15995 = CARTESIAN_POINT ( 'NONE',  ( -3.756430356249996105, 25.44062499938548427, 6.831223922626973533 ) ) ;
#15996 = EDGE_CURVE ( 'NONE', #11678, #10327, #12296, .T. ) ;
#15997 = CARTESIAN_POINT ( 'NONE',  ( 1.878215178125004048, -5.746835883940462963, 1.228124999385484584 ) ) ;
#15998 = CARTESIAN_POINT ( 'NONE',  ( 2.000000000000003997, -5.535898384862238508, 1.368749998770967702 ) ) ;
#15999 = CARTESIAN_POINT ( 'NONE',  ( 16.84448182151639628, 22.15687657743507089, 6.831223922626973533 ) ) ;
#16000 = CARTESIAN_POINT ( 'NONE',  ( -1.071796769724485676, 27.51115380933864074, 12.99999999999999467 ) ) ;
#16001 = VECTOR ( 'NONE', #647, 1000.000000000000000 ) ;
#16002 = ITEM_DEFINED_TRANSFORMATION ( 'NONE', 'NONE', #6445,  #21036 ) ;
#16003 = CARTESIAN_POINT ( 'NONE',  ( 3.752267015613588906E-15, 28.26250000000000284, 4.381197846482986158 ) ) ;
#16004 = EDGE_CURVE ( 'NONE', #22149, #10879, #12975, .T. ) ;
#16005 = CARTESIAN_POINT ( 'NONE',  ( -1.057460391440397258E-14, 29.16249999999999787, 4.999999999999992006 ) ) ;
#16006 = AXIS2_PLACEMENT_3D ( 'NONE', #8095, #5863, #3772 ) ;
#16007 = CARTESIAN_POINT ( 'NONE',  ( 23.66831732222138740, 18.35592256630256003, 11.16877607737301403 ) ) ;
#16008 = DIRECTION ( 'NONE',  ( 0.000000000000000000, 1.000000000000000000, 0.000000000000000000 ) ) ;
#16009 = ORIENTED_EDGE ( 'NONE', *, *, #4132, .F. ) ;
#16010 = ORIENTED_EDGE ( 'NONE', *, *, #25667, .T. ) ;
#16011 = CARTESIAN_POINT ( 'NONE',  ( -3.756430356249996105, 25.89062499938548356, 6.831223922626973533 ) ) ;
#16012 = ORIENTED_EDGE ( 'NONE', *, *, #24631, .T. ) ;
#16013 = CARTESIAN_POINT ( 'NONE',  ( -1.071796769724488563, 26.16115380933863221, 12.99999999999999289 ) ) ;
#16014 = AXIS2_PLACEMENT_3D ( 'NONE', #10509, #2289, #10635 ) ;
#16015 = CARTESIAN_POINT ( 'NONE',  ( 2.000000000000003997, 29.51874999877096784, 5.535898384862238508 ) ) ;
#16016 = CARTESIAN_POINT ( 'NONE',  ( 15.63147928073609982, 21.28833353022841379, 11.30940107675849404 ) ) ;
#16017 = DIRECTION ( 'NONE',  ( 1.000000000000000000, 0.000000000000000000, 0.000000000000000000 ) ) ;
#16018 = ORIENTED_EDGE ( 'NONE', *, *, #1500, .F. ) ;
#16019 = CIRCLE ( 'NONE', #18923, 0.5000000000000004441 ) ;
#16020 = CARTESIAN_POINT ( 'NONE',  ( 26.49999999999999645, 0.5000000000000000000, 19.50000000000000000 ) ) ;
#16021 = ORIENTED_EDGE ( 'NONE', *, *, #21544, .F. ) ;
#16022 = DIRECTION ( 'NONE',  ( 1.000000000000000000, 0.000000000000000000, 0.000000000000000000 ) ) ;
#16023 = CARTESIAN_POINT ( 'NONE',  ( 3.756430356250003655, 26.49062499938548498, 8.999999999999992895 ) ) ;
#16024 = CARTESIAN_POINT ( 'NONE',  ( -0.5000000000000000000, 0.000000000000000000, 19.50000000000000000 ) ) ;
#16025 = EDGE_CURVE ( 'NONE', #5115, #19269, #8298, .T. ) ;
#16026 = DIRECTION ( 'NONE',  ( 1.000000000000000000, 0.000000000000000000, 0.000000000000000000 ) ) ;
#16027 = CARTESIAN_POINT ( 'NONE',  ( 3.469446951953614189E-15, 46.00000000000000000, 3.499999999999992895 ) ) ;
#16028 = CARTESIAN_POINT ( 'NONE',  ( 4.000000000000007105, 25.93750000000000711, 6.690598923241489970 ) ) ;
#16029 = EDGE_CURVE ( 'NONE', #25447, #5108, #22905, .T. ) ;
#16030 = CARTESIAN_POINT ( 'NONE',  ( 2.672651547586948120E-15, 25.47812499938548569, 13.33755215474602984 ) ) ;
#16031 = EDGE_CURVE ( 'NONE', #22942, #21859, #14119, .T. ) ;
#16032 = CARTESIAN_POINT ( 'NONE',  ( -10.08469938919458286, 29.41953157733104263, -2.750000000000000000 ) ) ;
#16033 = SHAPE_REPRESENTATION ( 'casing', ( #21036 ), #8093 ) ;
#16034 = DIRECTION ( 'NONE',  ( -0.5877852522924775780, -0.8090169943749443426, 0.000000000000000000 ) ) ;
#16035 = CARTESIAN_POINT ( 'NONE',  ( -3.611812437532109232, 38.84323238218505736, 4.645898033750475165 ) ) ;
#16036 = CARTESIAN_POINT ( 'NONE',  ( 16.30765014111479516, 21.96450439060710380, 11.30940107675849404 ) ) ;
#16037 = CARTESIAN_POINT ( 'NONE',  ( 0.000000000000000000, 0.000000000000000000, -6.500000000000000000 ) ) ;
#16038 = ADVANCED_FACE ( 'NONE', ( #21057 ), #8904, .F. ) ;
#16039 = LINE ( 'NONE', #24000, #1745 ) ;
#16040 = CARTESIAN_POINT ( 'NONE',  ( 2.000000000000003997, 25.07499999999999929, 5.535898384862238508 ) ) ;
#16041 = CARTESIAN_POINT ( 'NONE',  ( 26.25859848311271705, 16.66421332384673804, -6.500000000000000000 ) ) ;
#16042 = CARTESIAN_POINT ( 'NONE',  ( 20.40224034548861809, 20.40224034548853993, 4.662447845253954171 ) ) ;
#16043 = ORIENTED_EDGE ( 'NONE', *, *, #1716, .T. ) ;
#16044 = CARTESIAN_POINT ( 'NONE',  ( 2.620986760973688460E-15, 27.53124999877097068, 13.61880215351699874 ) ) ;
#16045 = CARTESIAN_POINT ( 'NONE',  ( -3.752267015613588906E-15, -27.81250000000000000, 4.381197846482986158 ) ) ;
#16047 = ORIENTED_EDGE ( 'NONE', *, *, #4774, .T. ) ;
#16046 = CARTESIAN_POINT ( 'NONE',  ( -3.756430356250002323, 27.31562499938548783, 11.16877607737301048 ) ) ;
#16048 = CARTESIAN_POINT ( 'NONE',  ( -3.756430356249997438, 28.21562499938548640, 11.16877607737301048 ) ) ;
#16049 = DIRECTION ( 'NONE',  ( 0.000000000000000000, 0.000000000000000000, 1.000000000000000000 ) ) ;
#16050 = CARTESIAN_POINT ( 'NONE',  ( 28.72825533807133169, 11.91206721063041485, 1.000000000000000000 ) ) ;
#16051 = EDGE_LOOP ( 'NONE', ( #17743, #3634, #191, #6541 ) ) ;
#16052 = ORIENTED_EDGE ( 'NONE', *, *, #20649, .F. ) ;
#16053 = CARTESIAN_POINT ( 'NONE',  ( -3.756430356249994773, 28.06562499938548783, 8.999999999999992895 ) ) ;
#16054 = CARTESIAN_POINT ( 'NONE',  ( 4.000000000000001776, 28.05624999877096570, 11.30940107675849760 ) ) ;
#16055 = CARTESIAN_POINT ( 'NONE',  ( -3.756430356249996105, -6.831223922626973533, 3.478124999385480809 ) ) ;
#16056 = DIRECTION ( 'NONE',  ( -1.000000000000000000, 0.000000000000000000, 0.000000000000000000 ) ) ;
#16057 = PRESENTATION_STYLE_ASSIGNMENT (( #20090 ) ) ;
#16058 = CYLINDRICAL_SURFACE ( 'NONE', #14594, 30.00000000000000355 ) ;
#16059 = DIRECTION ( 'NONE',  ( 0.000000000000000000, 0.000000000000000000, 1.000000000000000000 ) ) ;
#16060 = LINE ( 'NONE', #2319, #19681 ) ;
#16061 = PRODUCT_DEFINITION_FORMATION_WITH_SPECIFIED_SOURCE ( 'ANY', '', #22379, .NOT_KNOWN. ) ;
#16062 = CARTESIAN_POINT ( 'NONE',  ( -3.999999999999996447, -8.999999999999992895, 4.275000000000001243 ) ) ;
#16063 = CARTESIAN_POINT ( 'NONE',  ( 20.62100150635272300, 20.62100150635266260, 4.999999999999992006 ) ) ;
#16064 = CARTESIAN_POINT ( 'NONE',  ( -3.959305671612554781E-15, -30.00000000000000355, 12.99999999999999289 ) ) ;
#16065 = CARTESIAN_POINT ( 'NONE',  ( 20.59006558380675855, 17.76163845906049943, 12.46410161513774817 ) ) ;
#16066 = ADVANCED_FACE ( 'NONE', ( #3137 ), #25236, .T. ) ;
#16067 = ORIENTED_EDGE ( 'NONE', *, *, #2225, .T. ) ;
#16068 = DIRECTION ( 'NONE',  ( -0.8090169943749417891, 0.5877852522924807976, 0.000000000000000000 ) ) ;
#16069 = DIRECTION ( 'NONE',  ( 1.000000000000000000, 0.000000000000000000, 0.000000000000000000 ) ) ;
#16070 = CARTESIAN_POINT ( 'NONE',  ( 1.878215178125000939, 29.67812499938548498, 12.25316411605952283 ) ) ;
#16071 = ADVANCED_FACE ( 'NONE', ( #19204 ), #8757, .T. ) ;
#16072 = CARTESIAN_POINT ( 'NONE',  ( -1.773386257881301553, 29.94852044693267246, 12.59496732558994125 ) ) ;
#16073 = DIRECTION ( 'NONE',  ( -6.938893903907225222E-15, -1.000000000000000000, 0.000000000000000000 ) ) ;
#16074 = CARTESIAN_POINT ( 'NONE',  ( 3.469446951953614189E-15, -8.999999999999992895, 18.00000000000000000 ) ) ;
#16075 = EDGE_LOOP ( 'NONE', ( #5451, #17556, #23456, #666 ) ) ;
#16076 = CARTESIAN_POINT ( 'NONE',  ( 1.071796769724492338, 27.10134618820329777, 12.99999999999999467 ) ) ;
#16077 = CARTESIAN_POINT ( 'NONE',  ( 25.99307600111999150, 0.5999999999999998668, 19.59999999999999787 ) ) ;
#16078 = CARTESIAN_POINT ( 'NONE',  ( -5.264710367730059737, 38.83395867543784163, 6.905309864513818674 ) ) ;
#16080 = ORIENTED_EDGE ( 'NONE', *, *, #18073, .T. ) ;
#16079 = DIRECTION ( 'NONE',  ( 0.000000000000000000, 0.000000000000000000, -1.000000000000000000 ) ) ;
#16081 = ORIENTED_EDGE ( 'NONE', *, *, #11122, .F. ) ;
#16082 = ORIENTED_EDGE ( 'NONE', *, *, #16724, .F. ) ;
#16083 = ORIENTED_EDGE ( 'NONE', *, *, #9829, .T. ) ;
#16084 = FACE_OUTER_BOUND ( 'NONE', #24046, .T. ) ;
#16085 = PLANE ( 'NONE',  #17225 ) ;
#16086 = CARTESIAN_POINT ( 'NONE',  ( 0.000000000000000000, 10.00000000000000000, 15.00000000000000178 ) ) ;
#16087 = CARTESIAN_POINT ( 'NONE',  ( 3.756430356250004987, 27.84062499938548640, 8.999999999999992895 ) ) ;
#16088 = CARTESIAN_POINT ( 'NONE',  ( -3.756430356249995661, -6.831223922626973533, 4.378124999385480720 ) ) ;
#16089 = CARTESIAN_POINT ( 'NONE',  ( 3.756430356250003655, -8.999999999999992895, 0.2531249993854844949 ) ) ;
#16090 = CARTESIAN_POINT ( 'NONE',  ( -3.756430356249996994, 26.26562499938548711, 8.999999999999992895 ) ) ;
#16091 = CARTESIAN_POINT ( 'NONE',  ( 3.469446951953614189E-15, 34.00000000000000000, 8.999999999999992895 ) ) ;
#16092 = CARTESIAN_POINT ( 'NONE',  ( -4.000000000000039968, -11.30940107675846740, 0.7124999999999979128 ) ) ;
#16093 = EDGE_CURVE ( 'NONE', #4544, #15602, #24850, .T. ) ;
#16094 = CARTESIAN_POINT ( 'NONE',  ( 1.878215178125000939, 27.31562499938548427, 12.25316411605952283 ) ) ;
#16095 = CYLINDRICAL_SURFACE ( 'NONE', #20052, 0.5000000000000004441 ) ;
#16096 = CARTESIAN_POINT ( 'NONE',  ( 1.999999999999995781, -25.54374999877096997, 5.535898384862237620 ) ) ;
#16097 = CARTESIAN_POINT ( 'NONE',  ( -28.72825533807142051, -11.91206721063020701, -6.500000000000000000 ) ) ;
#16098 = CARTESIAN_POINT ( 'NONE',  ( 1.999999999999995781, -29.59374999877096712, 5.535898384862237620 ) ) ;
#16099 = CARTESIAN_POINT ( 'NONE',  ( -1.878215178124995832, 29.00312499938548427, 5.746835883940462963 ) ) ;
#16100 = EDGE_CURVE ( 'NONE', #8164, #12818, #13311, .T. ) ;
#16101 = CARTESIAN_POINT ( 'NONE',  ( 0.000000000000000000, 0.000000000000000000, 19.50000000000000000 ) ) ;
#16102 = CARTESIAN_POINT ( 'NONE',  ( -3.999999999999995559, 29.63124999877096855, 6.690598923241487306 ) ) ;
#16103 = CYLINDRICAL_SURFACE ( 'NONE', #7228, 0.5000000000000004441 ) ;
#16104 = EDGE_LOOP ( 'NONE', ( #16980, #160, #1275, #15721, #11651, #6358 ) ) ;
#16105 = CARTESIAN_POINT ( 'NONE',  ( -3.999999999999998224, 27.02500000000000213, 8.999999999999992895 ) ) ;
#16107 = EDGE_LOOP ( 'NONE', ( #2281, #21280, #8578, #17873 ) ) ;
#16106 = CARTESIAN_POINT ( 'NONE',  ( -3.756430356250003655, -28.74062499938548498, 8.999999999999992895 ) ) ;
#16108 =( BOUNDED_CURVE ( )  B_SPLINE_CURVE ( 2, ( #2545, #12226, #6202, #10515, #22556, #8683, #24636 ),
 .UNSPECIFIED., .F., .F. ) 
 B_SPLINE_CURVE_WITH_KNOTS ( ( 3, 2, 2, 3 ),
 ( 0.4499999999999998446, 0.4666666666666665075, 0.4833333333333331150, 0.4999999999999997780 ),
 .UNSPECIFIED. ) 
 CURVE ( )  GEOMETRIC_REPRESENTATION_ITEM ( )  RATIONAL_B_SPLINE_CURVE ( ( 1.000000000000001332, 0.8660254037844373753, 1.000000000000000000, 0.8660254037844387076, 1.000000000000000000, 0.8660254037844404840, 0.9999999999999982236 ) ) 
 REPRESENTATION_ITEM ( '' )  );
#16109 = VERTEX_POINT ( 'NONE', #7051 ) ;
#16110 = ORIENTED_EDGE ( 'NONE', *, *, #24436, .F. ) ;
#16111 = ORIENTED_EDGE ( 'NONE', *, *, #2812, .F. ) ;
#16112 = ORIENTED_EDGE ( 'NONE', *, *, #460, .T. ) ;
#16113 = LINE ( 'NONE', #8258, #1715 ) ;
#16114 =( BOUNDED_CURVE ( )  B_SPLINE_CURVE ( 2, ( #2237, #12548, #20260, #10194, #274, #24188, #6659, #2742, #10448 ),
 .UNSPECIFIED., .F., .F. ) 
 B_SPLINE_CURVE_WITH_KNOTS ( ( 3, 2, 2, 2, 3 ),
 ( 0.1249999999999999861, 0.1333333333333333315, 0.1499999999999999944, 0.1666666666666666574, 0.1750000000000000167 ),
 .UNSPECIFIED. ) 
 CURVE ( )  GEOMETRIC_REPRESENTATION_ITEM ( )  RATIONAL_B_SPLINE_CURVE ( ( 0.9330127018922194093, 0.9330127018922192983, 1.000000000000000000, 0.8660254037844387076, 1.000000000000000000, 0.8660254037844387076, 1.000000000000000000, 0.9330127018922191873, 0.9330127018922194093 ) ) 
 REPRESENTATION_ITEM ( '' )  );
#16115 = EDGE_CURVE ( 'NONE', #15245, #25364, #9284, .T. ) ;
#16116 = VERTEX_POINT ( 'NONE', #15177 ) ;
#16117 = CARTESIAN_POINT ( 'NONE',  ( 2.000000000000003997, 29.12500000000000000, 5.535898384862238508 ) ) ;
#16118 = CARTESIAN_POINT ( 'NONE',  ( 1.878215178125000939, 26.97812499938548569, 12.25316411605952283 ) ) ;
#16119 = CARTESIAN_POINT ( 'NONE',  ( -1.878215178124995832, -5.746835883940462963, 2.203124999385484895 ) ) ;
#16120 = LINE ( 'NONE', #3957, #25032 ) ;
#16121 = PRODUCT_DEFINITION_SHAPE ( 'NONE', 'NONE',  #229 ) ;
#16122 = CARTESIAN_POINT ( 'NONE',  ( 18.65215106205190310, 18.65215106205183915, 13.33755215474602984 ) ) ;
#16123 = CARTESIAN_POINT ( 'NONE',  ( -1.453535542772288247, 31.06601413805604039, 1.000000000000000000 ) ) ;
#16124 = DIRECTION ( 'NONE',  ( 1.000000000000000000, 0.000000000000000000, 0.000000000000000000 ) ) ;
#16125 = CONTEXT_DEPENDENT_SHAPE_REPRESENTATION ( #9932, #1325 ) ;
#16126 = CARTESIAN_POINT ( 'NONE',  ( 2.672651547586948120E-15, -13.33755215474602984, 0.9281249993854824298 ) ) ;
#16127 = CARTESIAN_POINT ( 'NONE',  ( -1.999999999999998224, 28.44999999999999929, 12.46410161513774639 ) ) ;
#16128 = EDGE_CURVE ( 'NONE', #12209, #4122, #23146, .T. ) ;
#16129 = CARTESIAN_POINT ( 'NONE',  ( 4.000000000000003553, 29.08750000000000213, 6.690598923241489970 ) ) ;
#16130 = PLANE ( 'NONE',  #17158 ) ;
#16131 = CARTESIAN_POINT ( 'NONE',  ( 21.78337204305729458, 19.12717466509784003, 5.746835883940462963 ) ) ;
#16132 = DIRECTION ( 'NONE',  ( 1.000000000000000000, 0.000000000000000000, 0.000000000000000000 ) ) ;
#16133 = ORIENTED_EDGE ( 'NONE', *, *, #2336, .T. ) ;
#16134 = ORIENTED_EDGE ( 'NONE', *, *, #23660, .F. ) ;
#16135 = CARTESIAN_POINT ( 'NONE',  ( 4.000000000000001776, 29.89374999877097139, 8.999999999999992895 ) ) ;
#16136 = ADVANCED_FACE ( 'NONE', ( #22881 ), #5104, .F. ) ;
#16137 = EDGE_LOOP ( 'NONE', ( #24978, #9346, #17335, #8720 ) ) ;
#16138 = DIRECTION ( 'NONE',  ( 0.000000000000000000, -0.000000000000000000, 1.000000000000000000 ) ) ;
#16139 = CARTESIAN_POINT ( 'NONE',  ( 1.878215178125004048, 26.22812499938548569, 5.746835883940462963 ) ) ;
#16140 = CARTESIAN_POINT ( 'NONE',  ( 2.672651547586948120E-15, 29.64062499938548356, 13.33755215474602984 ) ) ;
#16141 = CARTESIAN_POINT ( 'NONE',  ( -3.999999999999973355, -6.690598923241474871, 2.381249998770965881 ) ) ;
#16142 = VERTEX_POINT ( 'NONE', #12692 ) ;
#16143 = ADVANCED_FACE ( 'NONE', ( #24718 ), #19081, .F. ) ;
#16144 = CYLINDRICAL_SURFACE ( 'NONE', #15700, 31.10000000000000142 ) ;
#16145 = EDGE_LOOP ( 'NONE', ( #20399, #11134 ) ) ;
#16146 = LINE ( 'NONE', #4767, #21424 ) ;
#16147 = CARTESIAN_POINT ( 'NONE',  ( -1.878215178124995832, 27.99062499938548143, 5.746835883940462963 ) ) ;
#16148 = CARTESIAN_POINT ( 'NONE',  ( 3.756430356250004987, 29.64062499938548711, 8.999999999999992895 ) ) ;
#16149 = CARTESIAN_POINT ( 'NONE',  ( 0.1556054994193530883, 38.97851006807006513, 3.480354713799856725 ) ) ;
#16150 = CARTESIAN_POINT ( 'NONE',  ( 1.859271017917182139E-15, 28.88124999877096499, 12.99999999999999289 ) ) ;
#16151 = CARTESIAN_POINT ( 'NONE',  ( -1.999999999999998224, 28.45000000000000639, 12.46410161513774639 ) ) ;
#16152 = FACE_OUTER_BOUND ( 'NONE', #11436, .T. ) ;
#16153 = FACE_OUTER_BOUND ( 'NONE', #8154, .T. ) ;
#16154 = LINE ( 'NONE', #18633, #12883 ) ;
#16155 = DIRECTION ( 'NONE',  ( 1.000000000000000000, 0.000000000000000000, 0.000000000000000000 ) ) ;
#16156 = CARTESIAN_POINT ( 'NONE',  ( 26.00000000000000711, 3.184081677783118980E-15, 20.00000000000000000 ) ) ;
#16157 = DIRECTION ( 'NONE',  ( 1.000000000000000000, 0.000000000000000000, 0.000000000000000000 ) ) ;
#16158 = CARTESIAN_POINT ( 'NONE',  ( -3.735045420075836212E-15, -25.25312499938548427, 4.662447845253954171 ) ) ;
#16159 = EDGE_CURVE ( 'NONE', #11855, #1614, #6804, .T. ) ;
#16160 = CARTESIAN_POINT ( 'NONE',  ( 5.337298091574883330, 38.72260848564139479, 11.21294222745710378 ) ) ;
#16161 = ORIENTED_EDGE ( 'NONE', *, *, #21628, .T. ) ;
#16162 = CARTESIAN_POINT ( 'NONE',  ( -3.999999999999996447, 28.76874999877096784, 8.999999999999992895 ) ) ;
#16163 = CARTESIAN_POINT ( 'NONE',  ( 3.999999999999997335, -28.86250000000000071, 11.30940107675849404 ) ) ;
#16165 = EDGE_LOOP ( 'NONE', ( #13020, #13887, #7477, #23566 ) ) ;
#16164 = CARTESIAN_POINT ( 'NONE',  ( 2.003086131649545506E-15, 27.39062499938549067, 13.33755215474603162 ) ) ;
#16166 = CARTESIAN_POINT ( 'NONE',  ( 3.756430356250003211, 28.89062499938548356, 6.831223922626973533 ) ) ;
#16167 = EDGE_CURVE ( 'NONE', #19798, #11078, #2868, .T. ) ;
#16168 = CARTESIAN_POINT ( 'NONE',  ( -1.071796769724481901, 27.96115380933863293, 12.99999999999999645 ) ) ;
#16169 = ORIENTED_EDGE ( 'NONE', *, *, #10752, .F. ) ;
#16170 = VERTEX_POINT ( 'NONE', #12815 ) ;
#16171 = CARTESIAN_POINT ( 'NONE',  ( 3.756430356250002323, 28.32812499938549067, 6.831223922626973533 ) ) ;
#16172 = CARTESIAN_POINT ( 'NONE',  ( 4.000000000000003553, 28.09374999877097068, 8.999999999999992895 ) ) ;
#16173 = CARTESIAN_POINT ( 'NONE',  ( -3.756430356249997438, -11.16877607737301048, 3.553124999385482763 ) ) ;
#16174 = EDGE_CURVE ( 'NONE', #16720, #16921, #4963, .T. ) ;
#16175 = DIRECTION ( 'NONE',  ( 0.000000000000000000, 0.000000000000000000, 1.000000000000000000 ) ) ;
#16176 = LINE ( 'NONE', #354, #10951 ) ;
#16177 = CARTESIAN_POINT ( 'NONE',  ( 1.859271017917182139E-15, 25.78750000000000142, 12.99999999999999289 ) ) ;
#16178 = FACE_OUTER_BOUND ( 'NONE', #1618, .T. ) ;
#16179 = CARTESIAN_POINT ( 'NONE',  ( 19.09750500040671284, 17.58175547255459747, 4.999999999999993783 ) ) ;
#16180 = CARTESIAN_POINT ( 'NONE',  ( 3.469446951953614189E-15, -8.999999999999992895, 18.00000000000000000 ) ) ;
#16182 = EDGE_CURVE ( 'NONE', #16109, #19025, #9456, .T. ) ;
#16181 = CARTESIAN_POINT ( 'NONE',  ( 16.57931677857143882, 21.89171153449011697, 11.16877607737301226 ) ) ;
#16183 = CARTESIAN_POINT ( 'NONE',  ( 22.72022476213123099, 17.06337051263877669, 6.690598923241489970 ) ) ;
#16184 = VERTEX_POINT ( 'NONE', #11748 ) ;
#16185 = FACE_OUTER_BOUND ( 'NONE', #15052, .T. ) ;
#16186 = FACE_OUTER_BOUND ( 'NONE', #10426, .T. ) ;
#16187 = CARTESIAN_POINT ( 'NONE',  ( 3.756430356250002323, 29.71562499938548640, 11.16877607737301226 ) ) ;
#16189 = VERTEX_POINT ( 'NONE', #9523 ) ;
#16188 = CARTESIAN_POINT ( 'NONE',  ( -3.871674220476135631, 29.74916513505594295, 7.961019890438434388 ) ) ;
#16190 = CARTESIAN_POINT ( 'NONE',  ( 18.87091222291601866, 18.87091222291595827, 12.99999999999999289 ) ) ;
#16191 = VERTEX_POINT ( 'NONE', #17647 ) ;
#16192 = DIRECTION ( 'NONE',  ( 0.000000000000000000, 0.000000000000000000, 1.000000000000000000 ) ) ;
#16193 = CARTESIAN_POINT ( 'NONE',  ( -31.00322564728516639, -2.451530025008796798, -2.750000000000000000 ) ) ;
#16194 = CARTESIAN_POINT ( 'NONE',  ( 1.878215178124995832, -27.09062499938548640, 5.746835883940462963 ) ) ;
#16196 = ORIENTED_EDGE ( 'NONE', *, *, #21594, .T. ) ;
#16195 = CARTESIAN_POINT ( 'NONE',  ( -29.72853858738287869, -9.133673601486284710, 1.000000000000000000 ) ) ;
#16197 = ORIENTED_EDGE ( 'NONE', *, *, #14086, .T. ) ;
#16198 = ORIENTED_EDGE ( 'NONE', *, *, #13607, .T. ) ;
#16199 = ORIENTED_EDGE ( 'NONE', *, *, #20025, .F. ) ;
#16200 = ADVANCED_FACE ( 'NONE', ( #3384 ), #5861, .T. ) ;
#16201 = CYLINDRICAL_SURFACE ( 'NONE', #22245, 31.10000000000000142 ) ;
#16202 = CARTESIAN_POINT ( 'NONE',  ( 9.133673601486471227, 29.72853858738282185, 1.000000000000000000 ) ) ;
#16203 = CIRCLE ( 'NONE', #2412, 0.5000000000000003331 ) ;
#16204 = CARTESIAN_POINT ( 'NONE',  ( -1.071796769724485454, 26.61115380933863150, 12.99999999999999467 ) ) ;
#16205 = ADVANCED_FACE ( 'NONE', ( #15558 ), #13328, .T. ) ;
#16206 = CARTESIAN_POINT ( 'NONE',  ( -1.878215178124998275, 28.14062499938548711, 12.25316411605951927 ) ) ;
#16207 = ADVANCED_FACE ( 'NONE', ( #17506 ), #19583, .T. ) ;
#16208 =( BOUNDED_CURVE ( )  B_SPLINE_CURVE ( 2, ( #10633, #12218, #14449, #710, #18625, #14326, #22289, #16660, #16418 ),
 .UNSPECIFIED., .F., .F. ) 
 B_SPLINE_CURVE_WITH_KNOTS ( ( 3, 2, 2, 2, 3 ),
 ( 0.3750000000000000000, 0.3833333333333333592, 0.4000000000000000222, 0.4166666666666666852, 0.4250000000000000444 ),
 .UNSPECIFIED. ) 
 CURVE ( )  GEOMETRIC_REPRESENTATION_ITEM ( )  RATIONAL_B_SPLINE_CURVE ( ( 0.9330127018922194093, 0.9330127018922194093, 1.000000000000000000, 0.8660254037844387076, 1.000000000000000000, 0.8660254037844387076, 1.000000000000000000, 0.9330127018922191873, 0.9330127018922194093 ) ) 
 REPRESENTATION_ITEM ( '' )  );
#16209 = AXIS2_PLACEMENT_3D ( 'NONE', #25133, #1335, #23421 ) ;
#16210 = CARTESIAN_POINT ( 'NONE',  ( -1.071796769724490561, 28.73259618943233207, 4.999999999999995559 ) ) ;
#16211 = CARTESIAN_POINT ( 'NONE',  ( -3.756430356249996994, -8.999999999999992895, 0.4781249993854840286 ) ) ;
#16212 = CARTESIAN_POINT ( 'NONE',  ( -3.756430356249997882, 26.75312499938548427, 11.16877607737301226 ) ) ;
#16213 = CARTESIAN_POINT ( 'NONE',  ( -3.137519842735244810E-15, 27.30624999877096926, 4.999999999999991118 ) ) ;
#16214 = CARTESIAN_POINT ( 'NONE',  ( -3.999999999999996447, -8.999999999999992895, 1.518749998770968501 ) ) ;
#16215 = CARTESIAN_POINT ( 'NONE',  ( 3.756430356250002323, 26.90312499938548285, 11.16877607737301403 ) ) ;
#16216 = DIRECTION ( 'NONE',  ( -0.7705132427757935831, -0.6374239897486843054, 0.000000000000000000 ) ) ;
#16217 = CARTESIAN_POINT ( 'NONE',  ( 31.03863125411925239, 1.952785157361540236, -6.500000000000000000 ) ) ;
#16218 = LINE ( 'NONE', #20380, #11798 ) ;
#16219 = CARTESIAN_POINT ( 'NONE',  ( -3.756430356250002323, -25.66562499938548569, 11.16877607737301226 ) ) ;
#16220 = CARTESIAN_POINT ( 'NONE',  ( 20.14370442905180525, 20.14370442905174130, 12.99999999999999289 ) ) ;
#16221 = CARTESIAN_POINT ( 'NONE',  ( 2.000000000000003997, -5.535898384862238508, 2.774999999999999467 ) ) ;
#16222 = VECTOR ( 'NONE', #16915, 1000.000000000000000 ) ;
#16223 = DIRECTION ( 'NONE',  ( 1.000000000000000000, 0.000000000000000000, 0.000000000000000000 ) ) ;
#16224 = CARTESIAN_POINT ( 'NONE',  ( 3.471149744654747238, -29.79887180468049479, 6.994934987683496530 ) ) ;
#16225 = ORIENTED_EDGE ( 'NONE', *, *, #22803, .F. ) ;
#16226 = CARTESIAN_POINT ( 'NONE',  ( -23.96296185032722548, -19.82388608118403539, -6.500000000000000000 ) ) ;
#16228 = ORIENTED_EDGE ( 'NONE', *, *, #25118, .T. ) ;
#16227 = DIRECTION ( 'NONE',  ( -0.000000000000000000, -0.000000000000000000, -1.000000000000000000 ) ) ;
#16229 = VECTOR ( 'NONE', #7096, 999.9999999999998863 ) ;
#16230 = VERTEX_POINT ( 'NONE', #7434 ) ;
#16232 = ORIENTED_EDGE ( 'NONE', *, *, #21869, .F. ) ;
#16231 = CIRCLE ( 'NONE', #15403, 0.5000000000000005551 ) ;
#16233 = EDGE_LOOP ( 'NONE', ( #8334, #19409 ) ) ;
#16234 = VERTEX_POINT ( 'NONE', #21438 ) ;
#16235 = CARTESIAN_POINT ( 'NONE',  ( 22.73348301514753800, 17.07662876565508370, 8.999999999999992895 ) ) ;
#16236 = ORIENTED_EDGE ( 'NONE', *, *, #1096, .T. ) ;
#16237 = EDGE_CURVE ( 'NONE', #18161, #20603, #9907, .T. ) ;
#16238 = CARTESIAN_POINT ( 'NONE',  ( 30.54913349766223973, 5.827558883615938434, -6.500000000000000000 ) ) ;
#16239 = CARTESIAN_POINT ( 'NONE',  ( -3.756430356249997438, 26.86562499938548498, 11.16877607737301048 ) ) ;
#16240 = EDGE_CURVE ( 'NONE', #51, #8668, #25616, .T. ) ;
#16241 = CIRCLE ( 'NONE', #4108, 31.10000000000000142 ) ;
#16242 = CARTESIAN_POINT ( 'NONE',  ( 1.878215178125004048, -5.746835883940462963, 3.478124999385483029 ) ) ;
#16243 = AXIS2_PLACEMENT_3D ( 'NONE', #20062, #11837, #6076 ) ;
#16244 = CARTESIAN_POINT ( 'NONE',  ( 2.000000000000000000, 25.82500000000000639, 12.46410161513774817 ) ) ;
#16245 = CARTESIAN_POINT ( 'NONE',  ( 19.79463422097012426, 17.13843684301067682, 5.746835883940462963 ) ) ;
#16246 = ADVANCED_FACE ( 'NONE', ( #7700 ), #21825, .F. ) ;
#16247 = CARTESIAN_POINT ( 'NONE',  ( 3.469446951953614189E-15, 38.49999999999999289, 8.999999999999992895 ) ) ;
#16248 = AXIS2_PLACEMENT_3D ( 'NONE', #14018, #2982, #14761 ) ;
#16249 = CARTESIAN_POINT ( 'NONE',  ( 0.000000000000000000, 6.000000000000000000, 19.50000000000000000 ) ) ;
#16250 = CIRCLE ( 'NONE', #24193, 31.10000000000000142 ) ;
#16251 = CARTESIAN_POINT ( 'NONE',  ( 2.672651547586948120E-15, -13.33755215474602984, 1.828124999385481786 ) ) ;
#16252 = CARTESIAN_POINT ( 'NONE',  ( 4.000000000000003553, -8.999999999999992895, 1.293749998770969079 ) ) ;
#16253 = CARTESIAN_POINT ( 'NONE',  ( 3.756430356250002323, 29.60312499938548569, 11.16877607737301403 ) ) ;
#16254 = CARTESIAN_POINT ( 'NONE',  ( -3.756430356249996994, -8.999999999999992895, 3.178124999385484983 ) ) ;
#16255 = CARTESIAN_POINT ( 'NONE',  ( -29.41953157733084012, 10.08469938919518327, 1.000000000000000000 ) ) ;
#16256 = CARTESIAN_POINT ( 'NONE',  ( -2.000000000000000888, -28.07500000000000284, 12.46410161513774817 ) ) ;
#16257 = ORIENTED_EDGE ( 'NONE', *, *, #7399, .T. ) ;
#16258 = ORIENTED_EDGE ( 'NONE', *, *, #25333, .T. ) ;
#16259 = CARTESIAN_POINT ( 'NONE',  ( -3.756430356249994329, 26.79062499938549280, 6.831223922626973533 ) ) ;
#16260 =( BOUNDED_CURVE ( )  B_SPLINE_CURVE ( 2, ( #10222, #9617, #5689, #22002, #4079, #16129, #6173, #14684, #12974 ),
 .UNSPECIFIED., .F., .F. ) 
 B_SPLINE_CURVE_WITH_KNOTS ( ( 3, 2, 2, 2, 3 ),
 ( 0.8750000000000000000, 0.8833333333333333037, 0.9000000000000000222, 0.9166666666666666297, 0.9250000000000000444 ),
 .UNSPECIFIED. ) 
 CURVE ( )  GEOMETRIC_REPRESENTATION_ITEM ( )  RATIONAL_B_SPLINE_CURVE ( ( 0.9330127018922194093, 0.9330127018922194093, 1.000000000000000000, 0.8660254037844387076, 1.000000000000000000, 0.8660254037844387076, 1.000000000000000000, 0.9330127018922189652, 0.9330127018922194093 ) ) 
 REPRESENTATION_ITEM ( '' )  );
#16262 = ORIENTED_EDGE ( 'NONE', *, *, #23753, .T. ) ;
#16261 = VECTOR ( 'NONE', #24463, 1000.000000000000000 ) ;
#16263 = PLANE ( 'NONE',  #13315 ) ;
#16264 = ORIENTED_EDGE ( 'NONE', *, *, #20808, .F. ) ;
#16265 = CARTESIAN_POINT ( 'NONE',  ( 19.41570305194066037, 17.89995352408853790, 4.999999999999992895 ) ) ;
#16266 = ORIENTED_EDGE ( 'NONE', *, *, #19003, .T. ) ;
#16267 = VECTOR ( 'NONE', #18362, 1000.000000000000000 ) ;
#16268 = DIRECTION ( 'NONE',  ( -0.000000000000000000, -0.000000000000000000, 1.000000000000000000 ) ) ;
#16269 = AXIS2_PLACEMENT_3D ( 'NONE', #16612, #4965, #10453 ) ;
#16270 = ORIENTED_EDGE ( 'NONE', *, *, #6855, .T. ) ;
#16271 = CARTESIAN_POINT ( 'NONE',  ( 2.000000000000000888, 28.46874999877097068, 12.46410161513774817 ) ) ;
#16272 = EDGE_CURVE ( 'NONE', #17199, #18353, #25498, .T. ) ;
#16273 = CARTESIAN_POINT ( 'NONE',  ( 3.756430356250004099, 26.52812499938548285, 6.831223922626973533 ) ) ;
#16274 = CARTESIAN_POINT ( 'NONE',  ( 0.000000000000000000, 29.52812499938548640, 13.33755215474603162 ) ) ;
#16275 = ADVANCED_FACE ( 'NONE', ( #7820 ), #15940, .F. ) ;
#16276 = VECTOR ( 'NONE', #1861, 1000.000000000000000 ) ;
#16277 = DIRECTION ( 'NONE',  ( -0.000000000000000000, 0.000000000000000000, -1.000000000000000000 ) ) ;
#16278 = LINE ( 'NONE', #4102, #16267 ) ;
#16279 = CARTESIAN_POINT ( 'NONE',  ( 4.000000000000005329, 29.05000000000000426, 8.999999999999992895 ) ) ;
#16280 = CIRCLE ( 'NONE', #21704, 0.5000000000000009992 ) ;
#16281 = AXIS2_PLACEMENT_3D ( 'NONE', #15183, #25243, #9290 ) ;
#16282 = CARTESIAN_POINT ( 'NONE',  ( -3.756430356249995661, 28.47812499938548569, 6.831223922626973533 ) ) ;
#16283 = VECTOR ( 'NONE', #6102, 1000.000000000000000 ) ;
#16284 = EDGE_CURVE ( 'NONE', #1590, #9464, #3684, .T. ) ;
#16285 = DIRECTION ( 'NONE',  ( 0.000000000000000000, -0.000000000000000000, 1.000000000000000000 ) ) ;
#16286 =( REPRESENTATION_RELATIONSHIP ('NONE','NONE', #25031, #20528 ) REPRESENTATION_RELATIONSHIP_WITH_TRANSFORMATION ( #19896 )SHAPE_REPRESENTATION_RELATIONSHIP( ) );
#16287 = CARTESIAN_POINT ( 'NONE',  ( 19.23330444827413643, 22.06173157302024634, 5.535898384862237620 ) ) ;
#16288 = LINE ( 'NONE', #24393, #20529 ) ;
#16289 = CARTESIAN_POINT ( 'NONE',  ( -30.63887302793240508, 5.335677986745117174, 1.000000000000000000 ) ) ;
#16290 = DIRECTION ( 'NONE',  ( -0.000000000000000000, -0.000000000000000000, 1.000000000000000000 ) ) ;
#16291 = CARTESIAN_POINT ( 'NONE',  ( 0.000000000000000000, 0.000000000000000000, -6.500000000000000000 ) ) ;
#16292 = CIRCLE ( 'NONE', #25466, 0.5000000000000001110 ) ;
#16293 = VERTEX_POINT ( 'NONE', #11362 ) ;
#16294 = CARTESIAN_POINT ( 'NONE',  ( 4.000000000000003553, 28.13124999877096855, 6.690598923241489970 ) ) ;
#16295 = DIRECTION ( 'NONE',  ( 0.000000000000000000, 0.000000000000000000, 1.000000000000000000 ) ) ;
#16297 = ORIENTED_EDGE ( 'NONE', *, *, #18847, .F. ) ;
#16296 = CARTESIAN_POINT ( 'NONE',  ( 1.878215178125008489, 27.57812499938549422, 5.746835883940462963 ) ) ;
#16298 = ORIENTED_EDGE ( 'NONE', *, *, #11312, .T. ) ;
#16299 = LINE ( 'NONE', #24267, #23344 ) ;
#16300 = VECTOR ( 'NONE', #20888, 1000.000000000000000 ) ;
#16301 = CARTESIAN_POINT ( 'NONE',  ( -3.401318489840788661, 30.91344420362550593, 1.000000000000000000 ) ) ;
#16302 = FACE_OUTER_BOUND ( 'NONE', #14285, .T. ) ;
#16303 = EDGE_LOOP ( 'NONE', ( #10178, #8039, #8919, #17282 ) ) ;
#16304 = ORIENTED_EDGE ( 'NONE', *, *, #9962, .T. ) ;
#16305 = CARTESIAN_POINT ( 'NONE',  ( 3.756430356249996105, -26.79062499938548569, 6.831223922626973533 ) ) ;
#16306 = CARTESIAN_POINT ( 'NONE',  ( 2.003086131649545506E-15, 29.07812499938549067, 13.33755215474602984 ) ) ;
#16307 = CYLINDRICAL_SURFACE ( 'NONE', #22655, 31.10000000000000142 ) ;
#16308 = COLOUR_RGB ( '',0.8941176470588234615, 0.8941176470588234615, 0.8941176470588234615 ) ;
#16309 = DIRECTION ( 'NONE',  ( 1.000000000000000000, 0.000000000000000000, 0.000000000000000000 ) ) ;
#16310 = AXIS2_PLACEMENT_3D ( 'NONE', #2009, #17334, #15497 ) ;
#16311 = EDGE_CURVE ( 'NONE', #2754, #414, #15812, .T. ) ;
#16312 = CARTESIAN_POINT ( 'NONE',  ( 3.526711513754840599, 38.89679573513954125, 4.645898033750303746 ) ) ;
#16313 = LINE ( 'NONE', #19713, #21276 ) ;
#16314 = CIRCLE ( 'NONE', #13388, 0.4999999999999996669 ) ;
#16315 = CIRCLE ( 'NONE', #4606, 4.000000000000000000 ) ;
#16316 = DIRECTION ( 'NONE',  ( 0.000000000000000000, 0.000000000000000000, 1.000000000000000000 ) ) ;
#16317 = CARTESIAN_POINT ( 'NONE',  ( -1.878215178124995832, 25.29062499938548569, 5.746835883940462963 ) ) ;
#16318 = CARTESIAN_POINT ( 'NONE',  ( 0.000000000000000000, 0.000000000000000000, -6.500000000000000000 ) ) ;
#16319 = CARTESIAN_POINT ( 'NONE',  ( 20.00801561637006643, 21.52376514422204323, 12.99999999999999289 ) ) ;
#16320 = CARTESIAN_POINT ( 'NONE',  ( 16.52628376998245230, 21.83867852590112690, 6.831223922626973533 ) ) ;
#16321 = CARTESIAN_POINT ( 'NONE',  ( 16.58607343533793710, 22.24292768483024929, 11.30940107675849404 ) ) ;
#16322 = ORIENTED_EDGE ( 'NONE', *, *, #10727, .F. ) ;
#16323 = CARTESIAN_POINT ( 'NONE',  ( 23.64116323484224225, -20.20656826142291251, -6.500000000000000000 ) ) ;
#16324 = CARTESIAN_POINT ( 'NONE',  ( 20.78010053211970032, 20.78010053211962926, 12.99999999999999289 ) ) ;
#16325 = CARTESIAN_POINT ( 'NONE',  ( -3.756430356249996994, 29.52812499938548640, 8.999999999999992895 ) ) ;
#16326 = AXIS2_PLACEMENT_3D ( 'NONE', #22054, #10027, #16059 ) ;
#16328 = ORIENTED_EDGE ( 'NONE', *, *, #11210, .T. ) ;
#16327 = DIRECTION ( 'NONE',  ( 1.000000000000000000, 0.000000000000000000, 0.000000000000000000 ) ) ;
#16329 = DIRECTION ( 'NONE',  ( -1.000000000000000000, 0.000000000000000000, 0.000000000000000000 ) ) ;
#16330 = CARTESIAN_POINT ( 'NONE',  ( 7.734255490826784651, -30.12293631110048153, 1.000000000000000000 ) ) ;
#16331 = ORIENTED_EDGE ( 'NONE', *, *, #25449, .T. ) ;
#16332 = DIRECTION ( 'NONE',  ( 1.000000000000000000, 0.000000000000000000, 0.000000000000000000 ) ) ;
#16333 = CARTESIAN_POINT ( 'NONE',  ( 2.000000000000000888, 26.66874999877096641, 12.46410161513774817 ) ) ;
#16334 = CARTESIAN_POINT ( 'NONE',  ( -3.756430356250003655, -26.49062499938548498, 8.999999999999992895 ) ) ;
#16336 = EDGE_LOOP ( 'NONE', ( #8348, #3194, #4033, #9799 ) ) ;
#16335 = CARTESIAN_POINT ( 'NONE',  ( -25.45105997952899912, 17.87326343783971083, -6.500000000000000000 ) ) ;
#16337 = CIRCLE ( 'NONE', #5052, 0.5000000000000001110 ) ;
#16338 = ORIENTED_EDGE ( 'NONE', *, *, #23410, .T. ) ;
#16339 = CARTESIAN_POINT ( 'NONE',  ( 1.878215178124995832, -29.45312499938548356, 5.746835883940462963 ) ) ;
#16340 = ORIENTED_EDGE ( 'NONE', *, *, #13347, .T. ) ;
#16341 = PRODUCT_DEFINITION_SHAPE ( 'NONE', 'NONE',  #24993 ) ;
#16342 = VERTEX_POINT ( 'NONE', #23526 ) ;
#16343 = CYLINDRICAL_SURFACE ( 'NONE', #112, 0.5000000000000004441 ) ;
#16344 = AXIS2_PLACEMENT_3D ( 'NONE', #16966, #6763, #12907 ) ;
#16345 = CARTESIAN_POINT ( 'NONE',  ( -3.756430356249996105, 26.41562499938548925, 11.16877607737301226 ) ) ;
#16346 = AXIS2_PLACEMENT_3D ( 'NONE', #24565, #6655, #24840 ) ;
#16347 = DIRECTION ( 'NONE',  ( -0.8090169943749498938, -0.5877852522924696954, 0.000000000000000000 ) ) ;
#16348 = VECTOR ( 'NONE', #14361, 1000.000000000000000 ) ;
#16349 = CARTESIAN_POINT ( 'NONE',  ( -5.706339097770935176, 31.50000000000000000, 7.145898033750358813 ) ) ;
#16350 = CARTESIAN_POINT ( 'NONE',  ( 3.735045420075836212E-15, -4.662447845253954171, 3.065624999385482052 ) ) ;
#16351 =( LENGTH_UNIT ( ) NAMED_UNIT ( * ) SI_UNIT ( .MILLI., .METRE. ) );
#16352 = CARTESIAN_POINT ( 'NONE',  ( -1.878215178124998497, 25.44062499938548427, 12.25316411605951927 ) ) ;
#16353 = EDGE_CURVE ( 'NONE', #12823, #5385, #24651, .T. ) ;
#16354 = CARTESIAN_POINT ( 'NONE',  ( 15.41874213889414591, 27.00874656207299651, -2.750000000000000000 ) ) ;
#16355 = CIRCLE ( 'NONE', #14263, 0.4999999999999997224 ) ;
#16356 = DIRECTION ( 'NONE',  ( 0.000000000000000000, 0.000000000000000000, 1.000000000000000000 ) ) ;
#16357 = CARTESIAN_POINT ( 'NONE',  ( 3.756430356250002323, 27.35312499938547859, 11.16877607737301403 ) ) ;
#16358 = CARTESIAN_POINT ( 'NONE',  ( 19.82388608118411710, -23.96296185032715798, -6.500000000000000000 ) ) ;
#16359 = CARTESIAN_POINT ( 'NONE',  ( 3.469446951953614189E-15, 25.00000000000000000, 8.999999999999992895 ) ) ;
#16360 = CARTESIAN_POINT ( 'NONE',  ( -1.859271017917182139E-15, -26.68750000000000000, 12.99999999999999289 ) ) ;
#16361 = EDGE_CURVE ( 'NONE', #7791, #19636, #19139, .T. ) ;
#16362 = CARTESIAN_POINT ( 'NONE',  ( -4.000000000000001776, -28.50624999877096855, 11.30940107675849760 ) ) ;
#16363 = AXIS2_PLACEMENT_3D ( 'NONE', #21561, #1693, #15685 ) ;
#16364 = CARTESIAN_POINT ( 'NONE',  ( -3.756430356249995661, 29.49062499938548498, 6.831223922626973533 ) ) ;
#16365 = VECTOR ( 'NONE', #18271, 1000.000000000000000 ) ;
#16366 = CARTESIAN_POINT ( 'NONE',  ( -1.999999999999995781, 27.85000000000000142, 5.535898384862237620 ) ) ;
#16367 = CARTESIAN_POINT ( 'NONE',  ( -22.32573188046889356, 21.65113613650366986, -6.500000000000000000 ) ) ;
#16368 = DIRECTION ( 'NONE',  ( 1.000000000000000000, 0.000000000000000000, 0.000000000000000000 ) ) ;
#16369 = ORIENTED_EDGE ( 'NONE', *, *, #25866, .T. ) ;
#16370 = EDGE_CURVE ( 'NONE', #18353, #21212, #14486, .T. ) ;
#16371 = DIRECTION ( 'NONE',  ( -0.000000000000000000, -0.000000000000000000, 1.000000000000000000 ) ) ;
#16373 = VERTEX_POINT ( 'NONE', #4152 ) ;
#16372 = DIRECTION ( 'NONE',  ( -0.000000000000000000, 0.000000000000000000, -1.000000000000000000 ) ) ;
#16374 = AXIS2_PLACEMENT_3D ( 'NONE', #9137, #4349, #20168 ) ;
#16375 = EDGE_LOOP ( 'NONE', ( #19175, #20041, #9950, #4758 ) ) ;
#16376 = ORIENTED_EDGE ( 'NONE', *, *, #17841, .T. ) ;
#16377 = ORIENTED_EDGE ( 'NONE', *, *, #5227, .F. ) ;
#16378 = ORIENTED_EDGE ( 'NONE', *, *, #13664, .F. ) ;
#16379 = ORIENTED_EDGE ( 'NONE', *, *, #20965, .T. ) ;
#16380 = CARTESIAN_POINT ( 'NONE',  ( -3.999999999999949818, -6.690598923241462437, 2.831249998770965615 ) ) ;
#16381 = AXIS2_PLACEMENT_3D ( 'NONE', #2820, #10184, #12285 ) ;
#16382 = ORIENTED_EDGE ( 'NONE', *, *, #5842, .T. ) ;
#16383 = DIRECTION ( 'NONE',  ( -0.000000000000000000, -0.000000000000000000, 1.000000000000000000 ) ) ;
#16384 = CARTESIAN_POINT ( 'NONE',  ( 3.735045420075836212E-15, 27.61562499938548498, 4.662447845253954171 ) ) ;
#16385 = VECTOR ( 'NONE', #19482, 1000.000000000000000 ) ;
#16386 = CARTESIAN_POINT ( 'NONE',  ( 3.756430356250003655, -8.999999999999992895, 2.503124999385482941 ) ) ;
#16387 = DIRECTION ( 'NONE',  ( 0.000000000000000000, 0.000000000000000000, 1.000000000000000000 ) ) ;
#16388 = CARTESIAN_POINT ( 'NONE',  ( 22.34249210749660364, 17.03009735157778337, 8.999999999999992895 ) ) ;
#16389 = VECTOR ( 'NONE', #8585, 1000.000000000000000 ) ;
#16390 = CARTESIAN_POINT ( 'NONE',  ( -22.67092431280609688, -21.28941499438201745, -6.500000000000000000 ) ) ;
#16391 = DIRECTION ( 'NONE',  ( -0.000000000000000000, 0.000000000000000000, 1.000000000000000000 ) ) ;
#16392 = CARTESIAN_POINT ( 'NONE',  ( -3.756430356249997882, -11.16877607737301226, 1.753124999385479832 ) ) ;
#16393 = CARTESIAN_POINT ( 'NONE',  ( 2.000000000000000888, -12.46410161513774817, 3.525000000000000355 ) ) ;
#16394 = CARTESIAN_POINT ( 'NONE',  ( -1.952785157361865753, -31.03863125411923463, -6.500000000000000000 ) ) ;
#16395 = CARTESIAN_POINT ( 'NONE',  ( 2.672651547586948120E-15, 29.07812499938548356, 13.33755215474603162 ) ) ;
#16396 = CARTESIAN_POINT ( 'NONE',  ( -3.756430356249996994, -8.999999999999992895, 2.728124999385482585 ) ) ;
#16397 = LINE ( 'NONE', #10342, #15957 ) ;
#16398 = DIRECTION ( 'NONE',  ( -0.000000000000000000, -0.000000000000000000, 1.000000000000000000 ) ) ;
#16399 = VECTOR ( 'NONE', #8644, 1000.000000000000000 ) ;
#16400 = EDGE_LOOP ( 'NONE', ( #18736, #7379, #20303, #12530 ) ) ;
#16401 = EDGE_CURVE ( 'NONE', #4731, #2838, #21234, .T. ) ;
#16402 = ORIENTED_EDGE ( 'NONE', *, *, #13888, .T. ) ;
#16403 = CARTESIAN_POINT ( 'NONE',  ( 3.756430356250006319, 27.99062499938548854, 6.831223922626973533 ) ) ;
#16404 = ADVANCED_FACE ( 'NONE', ( #12263 ), #8092, .F. ) ;
#16405 = ORIENTED_EDGE ( 'NONE', *, *, #9966, .F. ) ;
#16406 = FACE_OUTER_BOUND ( 'NONE', #577, .T. ) ;
#16407 = ORIENTED_EDGE ( 'NONE', *, *, #16934, .T. ) ;
#16408 = CARTESIAN_POINT ( 'NONE',  ( 8.831537335106614961E-15, 26.23749999999999716, 12.99999999999999112 ) ) ;
#16409 = ORIENTED_EDGE ( 'NONE', *, *, #13212, .F. ) ;
#16410 = CARTESIAN_POINT ( 'NONE',  ( 0.000000000000000000, 0.000000000000000000, 1.000000000000000000 ) ) ;
#16411 = EDGE_CURVE ( 'NONE', #5788, #25106, #9402, .T. ) ;
#16412 = CARTESIAN_POINT ( 'NONE',  ( 1.071796769724487230, -25.58259618943233704, 4.999999999999992006 ) ) ;
#16413 = EDGE_LOOP ( 'NONE', ( #23403, #21553, #18459, #16266 ) ) ;
#16414 = CYLINDRICAL_SURFACE ( 'NONE', #13090, 31.10000000000000142 ) ;
#16415 = CARTESIAN_POINT ( 'NONE',  ( -1.878215178124995832, 27.09062499938548640, 5.746835883940462963 ) ) ;
#16416 = DIRECTION ( 'NONE',  ( 0.000000000000000000, 0.000000000000000000, 1.000000000000000000 ) ) ;
#16417 = AXIS2_PLACEMENT_3D ( 'NONE', #20367, #12532, #6517 ) ;
#16418 = CARTESIAN_POINT ( 'NONE',  ( -3.137519842735244810E-15, 26.91249999999999787, 4.999999999999991118 ) ) ;
#16419 = CARTESIAN_POINT ( 'NONE',  ( 4.000000000000003553, 29.44374999877096855, 8.999999999999992895 ) ) ;
#16420 = CARTESIAN_POINT ( 'NONE',  ( 9.610428525060889626, 29.57785765677927614, -6.500000000000000000 ) ) ;
#16421 = AXIS2_PLACEMENT_3D ( 'NONE', #14194, #12227, #959 ) ;
#16422 = CARTESIAN_POINT ( 'NONE',  ( 3.735045420075836212E-15, 28.85312499938548569, 4.662447845253954171 ) ) ;
#16423 =( BOUNDED_CURVE ( )  B_SPLINE_CURVE ( 2, ( #15632, #1502, #23599, #3849, #11827, #1772, #9474 ),
 .UNSPECIFIED., .F., .F. ) 
 B_SPLINE_CURVE_WITH_KNOTS ( ( 3, 2, 2, 3 ),
 ( 0.8999999999999996891, 0.9166666666666665186, 0.9333333333333335702, 0.9500000000000003997 ),
 .UNSPECIFIED. ) 
 CURVE ( )  GEOMETRIC_REPRESENTATION_ITEM ( )  RATIONAL_B_SPLINE_CURVE ( ( 1.000000000000002665, 0.8660254037844360431, 1.000000000000000000, 0.8660254037844387076, 1.000000000000000000, 0.8660254037844351549, 1.000000000000003553 ) ) 
 REPRESENTATION_ITEM ( '' )  );
#16424 = FACE_OUTER_BOUND ( 'NONE', #5390, .T. ) ;
#16425 = CIRCLE ( 'NONE', #10151, 0.4999999999999998890 ) ;
#16426 = EDGE_CURVE ( 'NONE', #25364, #17650, #2433, .T. ) ;
#16427 = CARTESIAN_POINT ( 'NONE',  ( 18.70297436238422506, 21.53140148713034208, 12.46410161513774639 ) ) ;
#16428 = CARTESIAN_POINT ( 'NONE',  ( -1.999999999999998224, 29.35000000000000142, 12.46410161513774639 ) ) ;
#16429 = CARTESIAN_POINT ( 'NONE',  ( -10.94867358849371541, -28.91604871112453168, 1.000000000000000000 ) ) ;
#16431 = EDGE_CURVE ( 'NONE', #12726, #15349, #24295, .T. ) ;
#16430 = CARTESIAN_POINT ( 'NONE',  ( -3.999999999999995559, 25.18750000000000000, 6.690598923241487306 ) ) ;
#16432 = AXIS2_PLACEMENT_3D ( 'NONE', #23986, #12075, #8040 ) ;
#16433 = CARTESIAN_POINT ( 'NONE',  ( 21.65113613650327196, -22.32573188046928436, -6.500000000000000000 ) ) ;
#16434 = EDGE_LOOP ( 'NONE', ( #15843, #4978, #15620, #8640 ) ) ;
#16435 = CARTESIAN_POINT ( 'NONE',  ( -3.756430356249996994, 25.92812499938548498, 8.999999999999992895 ) ) ;
#16436 = CARTESIAN_POINT ( 'NONE',  ( -4.000000000000001776, -28.56249999999999645, 11.30940107675849760 ) ) ;
#16438 = ORIENTED_EDGE ( 'NONE', *, *, #11382, .F. ) ;
#16437 = CARTESIAN_POINT ( 'NONE',  ( 8.012344526598182026E-15, 28.51562499938548356, 4.662447845253954171 ) ) ;
#16439 = ORIENTED_EDGE ( 'NONE', *, *, #24073, .T. ) ;
#16440 = CARTESIAN_POINT ( 'NONE',  ( 1.999999999999998224, -29.29374999877096997, 12.46410161513774639 ) ) ;
#16441 = CYLINDRICAL_SURFACE ( 'NONE', #24675, 4.000000000000000000 ) ;
#16442 = CARTESIAN_POINT ( 'NONE',  ( 3.834746474454188013E-15, 27.75624999877096855, 4.999999999999992006 ) ) ;
#16443 = ORIENTED_EDGE ( 'NONE', *, *, #12659, .F. ) ;
#16444 = ORIENTED_EDGE ( 'NONE', *, *, #25140, .T. ) ;
#16445 = CARTESIAN_POINT ( 'NONE',  ( -3.756430356250003211, -25.74062499938548498, 6.831223922626973533 ) ) ;
#16446 = CARTESIAN_POINT ( 'NONE',  ( -3.756430356249996105, 28.47812499938548569, 6.831223922626973533 ) ) ;
#16447 = CARTESIAN_POINT ( 'NONE',  ( 2.000000000000000888, 28.01874999877096784, 12.46410161513774817 ) ) ;
#16448 = ADVANCED_FACE ( 'NONE', ( #631 ), #8598, .F. ) ;
#16449 = DIRECTION ( 'NONE',  ( 0.000000000000000000, 0.000000000000000000, 1.000000000000000000 ) ) ;
#16450 = AXIS2_PLACEMENT_3D ( 'NONE', #5224, #25235, #15292 ) ;
#16451 = VECTOR ( 'NONE', #6748, 1000.000000000000000 ) ;
#16452 = DIRECTION ( 'NONE',  ( 0.000000000000000000, 0.000000000000000000, 1.000000000000000000 ) ) ;
#16453 = CARTESIAN_POINT ( 'NONE',  ( -31.03863125411922752, 1.952785157361987878, -6.500000000000000000 ) ) ;
#16454 = LINE ( 'NONE', #4668, #9247 ) ;
#16455 = DIRECTION ( 'NONE',  ( -1.000000000000000000, 0.000000000000000000, 0.000000000000000000 ) ) ;
#16456 = CARTESIAN_POINT ( 'NONE',  ( 2.000000000000000888, 25.37500000000000000, 12.46410161513774817 ) ) ;
#16457 = CARTESIAN_POINT ( 'NONE',  ( 21.06969990136081705, 15.75730514544200211, 8.999999999999992895 ) ) ;
#16458 = CARTESIAN_POINT ( 'NONE',  ( 23.64830241243857500, 17.99144816294611715, 8.999999999999992895 ) ) ;
#16459 = FACE_OUTER_BOUND ( 'NONE', #3363, .T. ) ;
#16460 = CARTESIAN_POINT ( 'NONE',  ( 1.859271017917182139E-15, 26.18124999877096570, 12.99999999999999289 ) ) ;
#16461 = CARTESIAN_POINT ( 'NONE',  ( -3.756430356249995661, 25.32812499938548356, 6.831223922626973533 ) ) ;
#16463 = ORIENTED_EDGE ( 'NONE', *, *, #5556, .F. ) ;
#16462 = CARTESIAN_POINT ( 'NONE',  ( -1.774938052278379752, 29.94842879300231075, 5.405792698933810314 ) ) ;
#16464 = COLOUR_RGB ( '',0.8941176470588234615, 0.8941176470588234615, 0.8941176470588234615 ) ;
#16465 = CARTESIAN_POINT ( 'NONE',  ( 13.69242354489153080, 27.92360179968372691, -2.750000000000000000 ) ) ;
#16466 = DIRECTION ( 'NONE',  ( 1.000000000000000000, 0.000000000000000000, 0.000000000000000000 ) ) ;
#16467 = ORIENTED_EDGE ( 'NONE', *, *, #1394, .T. ) ;
#16468 = CARTESIAN_POINT ( 'NONE',  ( -3.137519842735244810E-15, 27.30624999877096926, 4.999999999999991118 ) ) ;
#16469 = CARTESIAN_POINT ( 'NONE',  ( -3.999999999999996003, 26.48124999877096641, 6.690598923241487306 ) ) ;
#16470 = CARTESIAN_POINT ( 'NONE',  ( 1.878215178124995832, -27.54062499938548214, 5.746835883940462963 ) ) ;
#16472 = ORIENTED_EDGE ( 'NONE', *, *, #11122, .T. ) ;
#16471 = CARTESIAN_POINT ( 'NONE',  ( 17.00591808753650724, 19.83434521228262426, 5.535898384862237620 ) ) ;
#16473 = PLANE ( 'NONE',  #16248 ) ;
#16474 = EDGE_CURVE ( 'NONE', #24372, #12662, #4024, .T. ) ;
#16475 = ORIENTED_EDGE ( 'NONE', *, *, #12460, .F. ) ;
#16476 = CARTESIAN_POINT ( 'NONE',  ( 3.756430356249996994, -25.81562499938548427, 8.999999999999992895 ) ) ;
#16477 = ORIENTED_EDGE ( 'NONE', *, *, #14746, .T. ) ;
#16478 = VERTEX_POINT ( 'NONE', #13174 ) ;
#16479 = CARTESIAN_POINT ( 'NONE',  ( -21.65113613650359525, -22.32573188046897172, -2.750000000000000000 ) ) ;
#16480 = CARTESIAN_POINT ( 'NONE',  ( -1.878215178124996498, 25.85312499938548925, 5.746835883940462963 ) ) ;
#16481 = LINE ( 'NONE', #22747, #8927 ) ;
#16482 = CARTESIAN_POINT ( 'NONE',  ( -3.756430356249996994, -8.999999999999992895, 2.278124999385483740 ) ) ;
#16483 =( NAMED_UNIT ( * ) PLANE_ANGLE_UNIT ( ) SI_UNIT ( $, .RADIAN. ) );
#16484 = FACE_OUTER_BOUND ( 'NONE', #21318, .T. ) ;
#16485 = CARTESIAN_POINT ( 'NONE',  ( 1.878215178125000939, 25.51562499938548356, 12.25316411605952283 ) ) ;
#16486 = CARTESIAN_POINT ( 'NONE',  ( 3.959305671612554781E-15, 35.50000000000000711, 12.99999999999999289 ) ) ;
#16487 = DIRECTION ( 'NONE',  ( 0.9685831611286337406, 0.2486898871648445808, 0.000000000000000000 ) ) ;
#16488 = CARTESIAN_POINT ( 'NONE',  ( 3.735045420075836212E-15, 25.70312499938548001, 4.662447845253954171 ) ) ;
#16489 = DIRECTION ( 'NONE',  ( 0.000000000000000000, 0.000000000000000000, 1.000000000000000000 ) ) ;
#16490 = DIRECTION ( 'NONE',  ( 1.000000000000000000, 0.000000000000000000, 0.000000000000000000 ) ) ;
#16491 = CARTESIAN_POINT ( 'NONE',  ( 3.752267015613588906E-15, -4.381197846482986158, 0.9562499987709653926 ) ) ;
#16492 = CARTESIAN_POINT ( 'NONE',  ( -1.878215178125004048, -27.12812499938548783, 5.746835883940462963 ) ) ;
#16493 = DIRECTION ( 'NONE',  ( 0.000000000000000000, -0.000000000000000000, 1.000000000000000000 ) ) ;
#16494 = DIRECTION ( 'NONE',  ( 1.000000000000000000, 0.000000000000000000, 0.000000000000000000 ) ) ;
#16495 = DIRECTION ( 'NONE',  ( 1.000000000000000000, 0.000000000000000000, 0.000000000000000000 ) ) ;
#16496 = CARTESIAN_POINT ( 'NONE',  ( -1.999999999999995781, 27.85000000000000142, 5.535898384862237620 ) ) ;
#16497 = ORIENTED_EDGE ( 'NONE', *, *, #9060, .T. ) ;
#16498 = CARTESIAN_POINT ( 'NONE',  ( 1.071796769724494114, 27.55134618820330061, 12.99999999999999112 ) ) ;
#16500 = VERTEX_POINT ( 'NONE', #11185 ) ;
#16499 = DIRECTION ( 'NONE',  ( 0.8660254037844397068, -0.4999999999999983347, 0.000000000000000000 ) ) ;
#16502 = ORIENTED_EDGE ( 'NONE', *, *, #4530, .F. ) ;
#16501 = EDGE_CURVE ( 'NONE', #9218, #16230, #3273, .T. ) ;
#16503 = ORIENTED_EDGE ( 'NONE', *, *, #13303, .T. ) ;
#16504 = EDGE_LOOP ( 'NONE', ( #20707, #4262, #4513, #19656 ) ) ;
#16505 = ORIENTED_EDGE ( 'NONE', *, *, #14968, .F. ) ;
#16506 = ORIENTED_EDGE ( 'NONE', *, *, #5206, .F. ) ;
#16507 = DIRECTION ( 'NONE',  ( -0.000000000000000000, -0.000000000000000000, 1.000000000000000000 ) ) ;
#16508 = ADVANCED_FACE ( 'NONE', ( #2711 ), #23113, .F. ) ;
#16509 = EDGE_LOOP ( 'NONE', ( #7168, #10911, #10356, #14465 ) ) ;
#16510 = EDGE_CURVE ( 'NONE', #23536, #11588, #14151, .T. ) ;
#16511 = DIRECTION ( 'NONE',  ( 0.000000000000000000, 0.000000000000000000, 1.000000000000000000 ) ) ;
#16512 = CARTESIAN_POINT ( 'NONE',  ( -26.50000000000000355, -0.5000000000000000000, 19.00000000000000000 ) ) ;
#16513 = CARTESIAN_POINT ( 'NONE',  ( -3.756430356249995661, -6.831223922626973533, 2.690624999385480276 ) ) ;
#16514 = CARTESIAN_POINT ( 'NONE',  ( -3.999999999999997335, -11.30940107675849404, 0.6562499987709655702 ) ) ;
#16515 = CARTESIAN_POINT ( 'NONE',  ( 16.26111872703749128, 21.57351348295617299, 11.16877607737301226 ) ) ;
#16516 = EDGE_CURVE ( 'NONE', #9980, #9464, #10812, .T. ) ;
#16517 = DIRECTION ( 'NONE',  ( 0.000000000000000000, -0.000000000000000000, -1.000000000000000000 ) ) ;
#16518 = CARTESIAN_POINT ( 'NONE',  ( 11.44867358849329619, -28.91604871112469510, 1.000000000000000000 ) ) ;
#16519 = CARTESIAN_POINT ( 'NONE',  ( 2.672651547586948120E-15, -13.33755215474602984, 2.728124999385481253 ) ) ;
#16520 = LINE ( 'NONE', #16032, #3348 ) ;
#16521 = CARTESIAN_POINT ( 'NONE',  ( 2.000000000000003997, -5.535898384862238508, 4.125000000000000000 ) ) ;
#16522 = CARTESIAN_POINT ( 'NONE',  ( -1.394453263437886604E-15, 27.30624999877096926, 4.999999999999991118 ) ) ;
#16523 = CARTESIAN_POINT ( 'NONE',  ( -1.878215178124998497, 28.59062499938548285, 12.25316411605951927 ) ) ;
#16524 = CARTESIAN_POINT ( 'NONE',  ( 1.878215178125000939, -12.25316411605952283, 1.528124999385482852 ) ) ;
#16525 = CARTESIAN_POINT ( 'NONE',  ( 1.071796769724495668, 27.55134618820330061, 12.99999999999999112 ) ) ;
#16526 = VERTEX_POINT ( 'NONE', #10673 ) ;
#16527 = VERTEX_POINT ( 'NONE', #22729 ) ;
#16528 = CARTESIAN_POINT ( 'NONE',  ( -3.756430356249994329, 28.59062499938548996, 6.831223922626973533 ) ) ;
#16529 = VERTEX_POINT ( 'NONE', #6624 ) ;
#16530 = DIRECTION ( 'NONE',  ( 1.000000000000000000, 0.000000000000000000, -0.000000000000000000 ) ) ;
#16531 = ORIENTED_EDGE ( 'NONE', *, *, #9891, .F. ) ;
#16532 = CARTESIAN_POINT ( 'NONE',  ( -3.999999999999996447, -8.999999999999992895, 2.418749998770966414 ) ) ;
#16533 = VERTEX_POINT ( 'NONE', #16968 ) ;
#16534 = LINE ( 'NONE', #12735, #12178 ) ;
#16535 = LINE ( 'NONE', #21323, #6918 ) ;
#16536 = ORIENTED_EDGE ( 'NONE', *, *, #13962, .F. ) ;
#16537 = DIRECTION ( 'NONE',  ( 0.000000000000000000, 0.000000000000000000, 1.000000000000000000 ) ) ;
#16538 = EDGE_CURVE ( 'NONE', #16142, #4937, #12061, .T. ) ;
#16539 = CARTESIAN_POINT ( 'NONE',  ( 3.756430356250002323, 26.90312499938548640, 11.16877607737301226 ) ) ;
#16540 = CARTESIAN_POINT ( 'NONE',  ( 3.878215178125001827, 25.07031249969274711, 8.999999999999992895 ) ) ;
#16541 = DIRECTION ( 'NONE',  ( 1.000000000000000000, 0.000000000000000000, 0.000000000000000000 ) ) ;
#16542 = CARTESIAN_POINT ( 'NONE',  ( 0.000000000000000000, 0.000000000000000000, -6.500000000000000000 ) ) ;
#16543 = DIRECTION ( 'NONE',  ( 1.000000000000000000, 0.000000000000000000, 0.000000000000000000 ) ) ;
#16544 = EDGE_CURVE ( 'NONE', #21567, #7608, #14876, .T. ) ;
#16545 = EDGE_CURVE ( 'NONE', #1492, #10494, #15422, .T. ) ;
#16546 = VECTOR ( 'NONE', #19219, 1000.000000000000000 ) ;
#16547 = CARTESIAN_POINT ( 'NONE',  ( -3.756430356249997882, 28.55312499938548498, 11.16877607737301226 ) ) ;
#16548 = CARTESIAN_POINT ( 'NONE',  ( 15.38607408531914089, 20.69846884123781550, 11.16877607737301048 ) ) ;
#16549 = CARTESIAN_POINT ( 'NONE',  ( 19.33937046545212013, 22.16779759019823359, 12.46410161513774639 ) ) ;
#16550 = CARTESIAN_POINT ( 'NONE',  ( 4.000000000000001776, 25.84374999877097423, 8.999999999999992895 ) ) ;
#16551 = CARTESIAN_POINT ( 'NONE',  ( 20.10392967174102097, 20.10392967174092860, 12.99999999999999289 ) ) ;
#16552 = CARTESIAN_POINT ( 'NONE',  ( 1.878215178124998497, -26.34062499938548285, 12.25316411605951927 ) ) ;
#16553 = CARTESIAN_POINT ( 'NONE',  ( -3.999999999999996447, -8.999999999999992895, 1.574999999999999956 ) ) ;
#16554 = EDGE_LOOP ( 'NONE', ( #23206, #16595, #8060, #1061 ) ) ;
#16555 = CARTESIAN_POINT ( 'NONE',  ( -1.999999999999998224, 29.74374999877096926, 12.46410161513774639 ) ) ;
#16556 = CARTESIAN_POINT ( 'NONE',  ( -4.000000000000003553, -29.05000000000000071, 8.999999999999992895 ) ) ;
#16558 = ORIENTED_EDGE ( 'NONE', *, *, #208, .F. ) ;
#16557 = CARTESIAN_POINT ( 'NONE',  ( -3.756430356249996549, 26.41562499938548925, 11.16877607737301048 ) ) ;
#16559 = ORIENTED_EDGE ( 'NONE', *, *, #3416, .T. ) ;
#16560 = CARTESIAN_POINT ( 'NONE',  ( -5.827558883616271501, -30.54913349766217934, -6.500000000000000000 ) ) ;
#16561 = CARTESIAN_POINT ( 'NONE',  ( 1.071796769724495446, 27.34240381056767433, 4.999999999999992895 ) ) ;
#16562 = ORIENTED_EDGE ( 'NONE', *, *, #16611, .T. ) ;
#16563 = CARTESIAN_POINT ( 'NONE',  ( -3.735045420075836212E-15, -27.61562499938548498, 4.662447845253954171 ) ) ;
#16564 = CARTESIAN_POINT ( 'NONE',  ( -1.878215178124998275, 28.59062499938548640, 12.25316411605951927 ) ) ;
#16565 = CARTESIAN_POINT ( 'NONE',  ( -1.071796769724487675, -29.08615380933863293, 4.999999999999988454 ) ) ;
#16566 = EDGE_CURVE ( 'NONE', #16529, #5616, #22596, .T. ) ;
#16567 = DIRECTION ( 'NONE',  ( 0.3090169943749456194, -0.9510565162951541973, 0.000000000000000000 ) ) ;
#16568 = EDGE_CURVE ( 'NONE', #6938, #10501, #21143, .T. ) ;
#16569 = LINE ( 'NONE', #10661, #19610 ) ;
#16570 = DIRECTION ( 'NONE',  ( 1.000000000000000000, 0.000000000000000000, 0.000000000000000000 ) ) ;
#16571 = CARTESIAN_POINT ( 'NONE',  ( 17.96051224213834985, 20.78893936688446331, 5.535898384862237620 ) ) ;
#16572 = CARTESIAN_POINT ( 'NONE',  ( -28.91604871112448549, 11.44867358849382910, 1.000000000000000000 ) ) ;
#16573 = CARTESIAN_POINT ( 'NONE',  ( 3.756430356250003655, 25.14062499938548356, 8.999999999999992895 ) ) ;
#16574 = CARTESIAN_POINT ( 'NONE',  ( 20.27186753227280747, 17.44344040752655545, 12.46410161513774817 ) ) ;
#16575 = CARTESIAN_POINT ( 'NONE',  ( 20.00676625532608455, 17.35056887736664422, 12.25316411605952283 ) ) ;
#16576 = CARTESIAN_POINT ( 'NONE',  ( 21.01432965251868978, 18.18590252777242711, 5.535898384862238508 ) ) ;
#16577 = CARTESIAN_POINT ( 'NONE',  ( 26.49999999999999645, 0.5000000000000000000, 19.50000000000000000 ) ) ;
#16578 = FACE_OUTER_BOUND ( 'NONE', #21270, .T. ) ;
#16579 = CARTESIAN_POINT ( 'NONE',  ( 3.756430356250002323, 25.55312499938548143, 11.16877607737301226 ) ) ;
#16581 = ORIENTED_EDGE ( 'NONE', *, *, #23161, .F. ) ;
#16580 = FACE_OUTER_BOUND ( 'NONE', #6837, .T. ) ;
#16582 = CARTESIAN_POINT ( 'NONE',  ( -0.5000000000000000000, -2.999999999999999556, 19.50000000000000000 ) ) ;
#16583 = CARTESIAN_POINT ( 'NONE',  ( -3.959305671612554781E-15, -30.00000000000000355, 12.99999999999999289 ) ) ;
#16584 = ORIENTED_EDGE ( 'NONE', *, *, #3402, .T. ) ;
#16585 = DIRECTION ( 'NONE',  ( -0.9297764858882481276, 0.3681245526846864125, 0.000000000000000000 ) ) ;
#16586 = CARTESIAN_POINT ( 'NONE',  ( 4.000000000000001776, 28.05624999877096926, 11.30940107675849760 ) ) ;
#16587 = CARTESIAN_POINT ( 'NONE',  ( -3.756430356250002323, -26.90312499938548640, 11.16877607737301226 ) ) ;
#16589 = EDGE_LOOP ( 'NONE', ( #844, #13786, #4693, #7028 ) ) ;
#16588 = CYLINDRICAL_SURFACE ( 'NONE', #17528, 31.10000000000000142 ) ;
#16590 = CARTESIAN_POINT ( 'NONE',  ( 27.25313774936419620, 14.98253926456328244, -6.500000000000000000 ) ) ;
#16591 = ORIENTED_EDGE ( 'NONE', *, *, #11468, .T. ) ;
#16593 = CARTESIAN_POINT ( 'NONE',  ( -2.672651547586948120E-15, -25.92812499938548498, 13.33755215474602984 ) ) ;
#16592 = ADVANCED_BREP_SHAPE_REPRESENTATION ( '', ( #4627, #21036 ), #23570 ) ;
#16594 = VERTEX_POINT ( 'NONE', #1014 ) ;
#16595 = ORIENTED_EDGE ( 'NONE', *, *, #16426, .F. ) ;
#16596 = DIRECTION ( 'NONE',  ( 1.000000000000000000, 0.000000000000000000, 0.000000000000000000 ) ) ;
#16597 = CARTESIAN_POINT ( 'NONE',  ( 4.000000000000003553, 27.73750000000000071, 6.690598923241489970 ) ) ;
#16598 = EDGE_CURVE ( 'NONE', #1524, #18550, #17915, .T. ) ;
#16599 = CARTESIAN_POINT ( 'NONE',  ( 3.756430356250002323, -11.16877607737301226, 2.015624999385483118 ) ) ;
#16600 = CARTESIAN_POINT ( 'NONE',  ( -1.878215178124995832, 26.19062499938548427, 5.746835883940462963 ) ) ;
#16601 = ADVANCED_FACE ( 'NONE', ( #16580 ), #4677, .F. ) ;
#16602 = DIRECTION ( 'NONE',  ( -0.06279051952930156388, 0.9980267284282724471, 0.000000000000000000 ) ) ;
#16603 = DIRECTION ( 'NONE',  ( 0.000000000000000000, 0.000000000000000000, 1.000000000000000000 ) ) ;
#16604 = CARTESIAN_POINT ( 'NONE',  ( 3.756430356250002323, 29.15312499938548640, 11.16877607737301403 ) ) ;
#16605 = FACE_OUTER_BOUND ( 'NONE', #7919, .T. ) ;
#16606 = CARTESIAN_POINT ( 'NONE',  ( 0.5000000000000000000, -2.999999999999999556, 19.50000000000000000 ) ) ;
#16607 = CARTESIAN_POINT ( 'NONE',  ( -3.999999999999996447, -8.999999999999992895, 1.068749998770966103 ) ) ;
#16608 = CARTESIAN_POINT ( 'NONE',  ( 3.756430356249995661, -27.24062499938548498, 6.831223922626973533 ) ) ;
#16609 = CARTESIAN_POINT ( 'NONE',  ( 3.735045420075836212E-15, 29.41562499938548569, 4.662447845253954171 ) ) ;
#16611 = EDGE_CURVE ( 'NONE', #18643, #25109, #12657, .T. ) ;
#16610 = DIRECTION ( 'NONE',  ( 0.000000000000000000, -1.000000000000000000, 0.000000000000000000 ) ) ;
#16612 = CARTESIAN_POINT ( 'NONE',  ( -28.91604871112448549, 11.44867358849382910, -6.500000000000000000 ) ) ;
#16613 = DIRECTION ( 'NONE',  ( 0.000000000000000000, -0.000000000000000000, -1.000000000000000000 ) ) ;
#16614 = VERTEX_POINT ( 'NONE', #12909 ) ;
#16615 = CARTESIAN_POINT ( 'NONE',  ( 13.69242354489133895, -27.92360179968382283, -6.500000000000000000 ) ) ;
#16617 = VERTEX_POINT ( 'NONE', #20756 ) ;
#16616 = DIRECTION ( 'NONE',  ( -0.000000000000000000, -0.000000000000000000, 1.000000000000000000 ) ) ;
#16618 = VERTEX_POINT ( 'NONE', #2834 ) ;
#16619 = VECTOR ( 'NONE', #23904, 1000.000000000000000 ) ;
#16620 = EDGE_LOOP ( 'NONE', ( #14210, #14495, #17945, #17360 ) ) ;
#16621 = ORIENTED_EDGE ( 'NONE', *, *, #11592, .F. ) ;
#16622 = ORIENTED_EDGE ( 'NONE', *, *, #17910, .F. ) ;
#16623 = CARTESIAN_POINT ( 'NONE',  ( 3.959305671612554781E-15, 40.00000000000000000, 12.99999999999999289 ) ) ;
#16624 = VERTEX_POINT ( 'NONE', #22851 ) ;
#16625 = DIRECTION ( 'NONE',  ( -0.000000000000000000, -1.000000000000000000, -0.000000000000000000 ) ) ;
#16626 = CARTESIAN_POINT ( 'NONE',  ( 1.878215178125000939, 27.87812499938548427, 12.25316411605952283 ) ) ;
#16627 = APPLICATION_CONTEXT ( 'automotive_design' ) ;
#16628 = CARTESIAN_POINT ( 'NONE',  ( 2.672651547586948120E-15, -13.33755215474602984, 3.740624999385483651 ) ) ;
#16629 = CARTESIAN_POINT ( 'NONE',  ( 20.56133937125558830, 20.56133937125551370, 13.33755215474602984 ) ) ;
#16630 = CARTESIAN_POINT ( 'NONE',  ( 10.98232076577200722, -29.09636799667087459, -2.750000000000000000 ) ) ;
#16631 = ADVANCED_FACE ( 'NONE', ( #10802 ), #8866, .T. ) ;
#16632 = DIRECTION ( 'NONE',  ( -0.9297764858882532346, -0.3681245526846732008, 0.000000000000000000 ) ) ;
#16633 = AXIS2_PLACEMENT_3D ( 'NONE', #25650, #12022, #21473 ) ;
#16634 = CARTESIAN_POINT ( 'NONE',  ( -3.756430356249995661, -6.831223922626973533, 1.228124999385478144 ) ) ;
#16635 = CYLINDRICAL_SURFACE ( 'NONE', #24223, 0.5000000000000004441 ) ;
#16636 = CARTESIAN_POINT ( 'NONE',  ( -3.999999999999996003, -6.690598923241487306, 3.337499999999999023 ) ) ;
#16637 = CARTESIAN_POINT ( 'NONE',  ( 6.938893903907228378E-15, 31.50000000000000000, 3.499999999999992450 ) ) ;
#16638 = CARTESIAN_POINT ( 'NONE',  ( 19.43607991388971712, -24.27856662945514543, -2.750000000000000000 ) ) ;
#16639 =( BOUNDED_CURVE ( )  B_SPLINE_CURVE ( 2, ( #11702, #5813, #7906, #5953, #17728, #14059, #6560 ),
 .UNSPECIFIED., .F., .F. ) 
 B_SPLINE_CURVE_WITH_KNOTS ( ( 3, 2, 2, 3 ),
 ( 0.000000000000000000, 0.01666666666666663521, 0.03333333333333327042, 0.04999999999999990563 ),
 .UNSPECIFIED. ) 
 CURVE ( )  GEOMETRIC_REPRESENTATION_ITEM ( )  RATIONAL_B_SPLINE_CURVE ( ( 1.000000000000000000, 0.8660254037844387076, 1.000000000000000000, 0.8660254037844387076, 1.000000000000000000, 0.8660254037844394848, 0.9999999999999992228 ) ) 
 REPRESENTATION_ITEM ( '' )  );
#16640 = CARTESIAN_POINT ( 'NONE',  ( 3.756430356250003655, -8.999999999999992895, 1.153124999385485960 ) ) ;
#16641 = DIRECTION ( 'NONE',  ( 1.000000000000000000, 0.000000000000000000, 0.000000000000000000 ) ) ;
#16642 = AXIS2_PLACEMENT_3D ( 'NONE', #20562, #8931, #8789 ) ;
#16643 = DIRECTION ( 'NONE',  ( -0.000000000000000000, -1.000000000000000000, -0.000000000000000000 ) ) ;
#16644 = ORIENTED_EDGE ( 'NONE', *, *, #8244, .T. ) ;
#16645 = ORIENTED_EDGE ( 'NONE', *, *, #12222, .F. ) ;
#16646 = CARTESIAN_POINT ( 'NONE',  ( -1.878215178124998275, 28.10312499938548925, 5.746835883940462963 ) ) ;
#16647 = VERTEX_POINT ( 'NONE', #13045 ) ;
#16648 = CARTESIAN_POINT ( 'NONE',  ( 28.91604871112465602, 11.44867358849340633, -6.500000000000000000 ) ) ;
#16649 = ORIENTED_EDGE ( 'NONE', *, *, #4303, .T. ) ;
#16650 = CARTESIAN_POINT ( 'NONE',  ( 1.878215178124995832, -25.40312499938548640, 5.746835883940462963 ) ) ;
#16651 = ORIENTED_EDGE ( 'NONE', *, *, #2772, .T. ) ;
#16652 = CARTESIAN_POINT ( 'NONE',  ( 3.959305671612554781E-15, 35.50000000000000711, 12.99999999999999289 ) ) ;
#16653 = AXIS2_PLACEMENT_3D ( 'NONE', #9020, #7192, #17003 ) ;
#16654 = EDGE_LOOP ( 'NONE', ( #20667, #18419, #15463, #24721 ) ) ;
#16655 = AXIS2_PLACEMENT_3D ( 'NONE', #18788, #875, #7396 ) ;
#16656 = CYLINDRICAL_SURFACE ( 'NONE', #13925, 4.000000000000000000 ) ;
#16657 = CARTESIAN_POINT ( 'NONE',  ( -3.756430356249997882, 29.00312499938548072, 11.16877607737301226 ) ) ;
#16658 = CARTESIAN_POINT ( 'NONE',  ( 2.000000000000000888, 27.11874999877096926, 12.46410161513774817 ) ) ;
#16659 = AXIS2_PLACEMENT_3D ( 'NONE', #3946, #19769, #1864 ) ;
#16660 = CARTESIAN_POINT ( 'NONE',  ( 1.071796769724491227, 26.89240381056766793, 4.999999999999989342 ) ) ;
#16661 = DIRECTION ( 'NONE',  ( -1.000000000000000000, 0.000000000000000000, 0.000000000000000000 ) ) ;
#16662 = EDGE_CURVE ( 'NONE', #18727, #16889, #10636, .T. ) ;
#16663 = CARTESIAN_POINT ( 'NONE',  ( 22.10384356884614121, 16.79144881292732450, 8.999999999999992895 ) ) ;
#16664 = CARTESIAN_POINT ( 'NONE',  ( 3.756430356250003655, 26.94062499938548427, 8.999999999999992895 ) ) ;
#16665 = EDGE_CURVE ( 'NONE', #10805, #7768, #9625, .T. ) ;
#16666 = DIRECTION ( 'NONE',  ( -0.000000000000000000, 0.000000000000000000, 1.000000000000000000 ) ) ;
#16667 = VECTOR ( 'NONE', #21107, 1000.000000000000000 ) ;
#16668 = CARTESIAN_POINT ( 'NONE',  ( 20.62100150635273366, 20.62100150635265905, 4.381197846482986158 ) ) ;
#16669 = ADVANCED_FACE ( 'NONE', ( #7285 ), #5443, .T. ) ;
#16670 = CARTESIAN_POINT ( 'NONE',  ( -3.999999999999999556, 26.10624999877097352, 11.30940107675849404 ) ) ;
#16671 = CARTESIAN_POINT ( 'NONE',  ( 3.469446951953614189E-15, 31.50000000000000000, 4.999999999999992006 ) ) ;
#16673 = CARTESIAN_POINT ( 'NONE',  ( -1.878215178125004048, -27.01562499938548711, 5.746835883940462963 ) ) ;
#16672 = VECTOR ( 'NONE', #16717, 1000.000000000000000 ) ;
#16674 = CARTESIAN_POINT ( 'NONE',  ( 5.244320908822881933, 38.86762122992235646, 11.05479723877108178 ) ) ;
#16675 = VECTOR ( 'NONE', #18665, 1000.000000000000000 ) ;
#16676 = VERTEX_POINT ( 'NONE', #19430 ) ;
#16677 = CARTESIAN_POINT ( 'NONE',  ( 1.878215178125000939, 26.07812499938548356, 12.25316411605952283 ) ) ;
#16678 = LINE ( 'NONE', #6087, #2104 ) ;
#16679 = EDGE_CURVE ( 'NONE', #10674, #23645, #10275, .T. ) ;
#16681 = ORIENTED_EDGE ( 'NONE', *, *, #14746, .F. ) ;
#16680 = CARTESIAN_POINT ( 'NONE',  ( 0.000000000000000000, 0.000000000000000000, 1.000000000000000000 ) ) ;
#16682 = VERTEX_POINT ( 'NONE', #13435 ) ;
#16683 = DIRECTION ( 'NONE',  ( -0.000000000000000000, -1.000000000000000000, -0.000000000000000000 ) ) ;
#16684 = CARTESIAN_POINT ( 'NONE',  ( -3.999999999999996447, -8.999999999999992895, 0.6187499987709670357 ) ) ;
#16685 = ORIENTED_EDGE ( 'NONE', *, *, #4093, .F. ) ;
#16686 = CARTESIAN_POINT ( 'NONE',  ( 3.756430356249997438, -26.86562499938548498, 11.16877607737301048 ) ) ;
#16687 = DIRECTION ( 'NONE',  ( 0.000000000000000000, 1.000000000000000000, 0.000000000000000000 ) ) ;
#16688 = CARTESIAN_POINT ( 'NONE',  ( -3.756430356249996549, 25.36562499938548854, 8.999999999999992895 ) ) ;
#16689 = AXIS2_PLACEMENT_3D ( 'NONE', #9482, #19161, #9615 ) ;
#16690 = CIRCLE ( 'NONE', #4561, 31.10000000000000142 ) ;
#16691 = FACE_OUTER_BOUND ( 'NONE', #632, .T. ) ;
#16692 = CARTESIAN_POINT ( 'NONE',  ( -3.756430356249996105, 26.22812499938548569, 6.831223922626973533 ) ) ;
#16693 = CIRCLE ( 'NONE', #21284, 0.4999999999999995004 ) ;
#16694 = VECTOR ( 'NONE', #16138, 1000.000000000000000 ) ;
#16695 = CARTESIAN_POINT ( 'NONE',  ( 3.469446951953614189E-15, 40.00000000000000000, 8.999999999999992895 ) ) ;
#16696 = FACE_OUTER_BOUND ( 'NONE', #21896, .T. ) ;
#16697 = DIRECTION ( 'NONE',  ( 0.000000000000000000, 0.000000000000000000, 1.000000000000000000 ) ) ;
#16698 = DIRECTION ( 'NONE',  ( -0.000000000000000000, -0.000000000000000000, -1.000000000000000000 ) ) ;
#16699 = CIRCLE ( 'NONE', #10401, 4.000000000000000000 ) ;
#16700 = DIRECTION ( 'NONE',  ( 0.000000000000000000, 0.000000000000000000, 1.000000000000000000 ) ) ;
#16701 = CARTESIAN_POINT ( 'NONE',  ( 21.27955846146187113, 18.62336108350243080, 12.25316411605952283 ) ) ;
#16702 = CARTESIAN_POINT ( 'NONE',  ( 20.85756786700484966, 15.54517311108603472, 6.831223922626973533 ) ) ;
#16703 = FACE_OUTER_BOUND ( 'NONE', #21184, .T. ) ;
#16704 = CARTESIAN_POINT ( 'NONE',  ( 3.469446951953614189E-15, -8.999999999999992895, 18.00000000000000000 ) ) ;
#16705 = CARTESIAN_POINT ( 'NONE',  ( 1.878215178125000939, 28.66562499938548569, 12.25316411605952283 ) ) ;
#16706 = CIRCLE ( 'NONE', #7514, 0.4999999999999991118 ) ;
#16708 = VERTEX_POINT ( 'NONE', #7402 ) ;
#16707 = CARTESIAN_POINT ( 'NONE',  ( -30.12293631110035363, 7.734255490827311341, -6.500000000000000000 ) ) ;
#16709 = CARTESIAN_POINT ( 'NONE',  ( -8.217531866530787710, 29.99470236596041772, -6.500000000000000000 ) ) ;
#16710 = ORIENTED_EDGE ( 'NONE', *, *, #13314, .F. ) ;
#16711 = DIRECTION ( 'NONE',  ( 0.000000000000000000, 0.000000000000000000, 1.000000000000000000 ) ) ;
#16712 = CARTESIAN_POINT ( 'NONE',  ( -3.999999999999997335, 27.90624999877097068, 11.30940107675849404 ) ) ;
#16713 = CARTESIAN_POINT ( 'NONE',  ( 1.878215178124998497, -25.44062499938548427, 12.25316411605951927 ) ) ;
#16714 = EDGE_CURVE ( 'NONE', #16527, #7608, #5791, .T. ) ;
#16716 = ORIENTED_EDGE ( 'NONE', *, *, #20753, .T. ) ;
#16715 = DIRECTION ( 'NONE',  ( 0.000000000000000000, 0.000000000000000000, 1.000000000000000000 ) ) ;
#16717 = DIRECTION ( 'NONE',  ( 1.000000000000000000, 0.000000000000000000, 0.000000000000000000 ) ) ;
#16719 = ADVANCED_FACE ( 'NONE', ( #23616 ), #23230, .F. ) ;
#16718 = CIRCLE ( 'NONE', #2918, 0.5000000000000002220 ) ;
#16720 = VERTEX_POINT ( 'NONE', #9376 ) ;
#16721 = CARTESIAN_POINT ( 'NONE',  ( 3.756430356249997882, -29.56562499938549138, 11.16877607737301226 ) ) ;
#16722 = ORIENTED_EDGE ( 'NONE', *, *, #19586, .T. ) ;
#16723 = ORIENTED_EDGE ( 'NONE', *, *, #16272, .T. ) ;
#16724 = EDGE_CURVE ( 'NONE', #12847, #337, #17473, .T. ) ;
#16725 = CARTESIAN_POINT ( 'NONE',  ( 1.878215178125001605, 27.42812499938548854, 12.25316411605952283 ) ) ;
#16726 = ADVANCED_FACE ( 'NONE', ( #5822 ), #13558, .T. ) ;
#16727 = AXIS2_PLACEMENT_3D ( 'NONE', #7320, #9024, #15300 ) ;
#16728 = CARTESIAN_POINT ( 'NONE',  ( 4.000000000000003553, -8.999999999999992895, 3.543749998770967302 ) ) ;
#16729 = CIRCLE ( 'NONE', #858, 31.10000000000000142 ) ;
#16730 = VECTOR ( 'NONE', #18168, 1000.000000000000000 ) ;
#16731 = ADVANCED_FACE ( 'NONE', ( #9490 ), #7528, .T. ) ;
#16732 = CARTESIAN_POINT ( 'NONE',  ( 3.756430356250003655, -8.999999999999992895, 1.153124999385485960 ) ) ;
#16733 = PRESENTATION_STYLE_ASSIGNMENT (( #6912 ) ) ;
#16734 = LINE ( 'NONE', #14775, #14712 ) ;
#16735 = CARTESIAN_POINT ( 'NONE',  ( 1.878215178125004048, 27.91562499938548569, 5.746835883940462963 ) ) ;
#16736 = CIRCLE ( 'NONE', #12964, 0.5000000000000002220 ) ;
#16737 = DIRECTION ( 'NONE',  ( 0.000000000000000000, -1.000000000000000000, 0.000000000000000000 ) ) ;
#16738 = CARTESIAN_POINT ( 'NONE',  ( -14.98253926456298579, 27.25313774936435962, -6.500000000000000000 ) ) ;
#16739 = UNCERTAINTY_MEASURE_WITH_UNIT (LENGTH_MEASURE( 1.000000000000000082E-05 ), #16351, 'distance_accuracy_value', 'NONE');
#16740 = CARTESIAN_POINT ( 'NONE',  ( 1.878215178125004048, 27.91562499938548569, 5.746835883940462963 ) ) ;
#16741 = DIRECTION ( 'NONE',  ( 0.000000000000000000, 0.000000000000000000, 1.000000000000000000 ) ) ;
#16742 = CARTESIAN_POINT ( 'NONE',  ( 23.14903047711951345, 19.08292775625380600, 11.79623638833883881 ) ) ;
#16743 = DIRECTION ( 'NONE',  ( -0.9822872507286897203, -0.1873813145857189666, 0.000000000000000000 ) ) ;
#16744 = CARTESIAN_POINT ( 'NONE',  ( -3.756430356250003655, -27.50312499938548427, 8.999999999999992895 ) ) ;
#16745 = CARTESIAN_POINT ( 'NONE',  ( 23.01025686871637177, 20.92219106202051293, 1.000000000000000000 ) ) ;
#16746 = CARTESIAN_POINT ( 'NONE',  ( -27.10000000000000497, -0.5999999999999998668, 19.59999999999999787 ) ) ;
#16747 = VECTOR ( 'NONE', #18734, 1000.000000000000000 ) ;
#16748 = CYLINDRICAL_SURFACE ( 'NONE', #7486, 0.5000000000000004441 ) ;
#16749 = CARTESIAN_POINT ( 'NONE',  ( 3.834746474454188013E-15, 27.81249999999999645, 4.999999999999992006 ) ) ;
#16750 = ORIENTED_EDGE ( 'NONE', *, *, #16284, .F. ) ;
#16751 = LINE ( 'NONE', #2488, #23378 ) ;
#16753 = ORIENTED_EDGE ( 'NONE', *, *, #12112, .T. ) ;
#16752 = DIRECTION ( 'NONE',  ( 0.000000000000000000, 1.000000000000000000, 0.000000000000000000 ) ) ;
#16754 = AXIS2_PLACEMENT_3D ( 'NONE', #8474, #20883, #8717 ) ;
#16755 = EDGE_CURVE ( 'NONE', #7506, #7412, #6943, .T. ) ;
#16756 = AXIS2_PLACEMENT_3D ( 'NONE', #20914, #22873, #1039 ) ;
#16757 = VERTEX_POINT ( 'NONE', #3994 ) ;
#16758 = ORIENTED_EDGE ( 'NONE', *, *, #12674, .F. ) ;
#16759 = ORIENTED_EDGE ( 'NONE', *, *, #19420, .F. ) ;
#16760 = ORIENTED_EDGE ( 'NONE', *, *, #24725, .F. ) ;
#16761 = VECTOR ( 'NONE', #2561, 1000.000000000000000 ) ;
#16762 = CARTESIAN_POINT ( 'NONE',  ( -2.000000000000000888, -27.62500000000000000, 12.46410161513774817 ) ) ;
#16763 = AXIS2_PLACEMENT_3D ( 'NONE', #12155, #21969, #8364 ) ;
#16764 = ORIENTED_EDGE ( 'NONE', *, *, #13772, .T. ) ;
#16765 = DIRECTION ( 'NONE',  ( 0.000000000000000000, -1.000000000000000000, -0.000000000000000000 ) ) ;
#16766 = CARTESIAN_POINT ( 'NONE',  ( -1.878215178124995832, 29.45312499938548356, 5.746835883940462963 ) ) ;
#16767 = EDGE_CURVE ( 'NONE', #3783, #18040, #12093, .T. ) ;
#16768 = VECTOR ( 'NONE', #16277, 1000.000000000000000 ) ;
#16769 = CARTESIAN_POINT ( 'NONE',  ( 3.756430356250002323, -11.16877607737301226, 4.265624999385481786 ) ) ;
#16770 = CARTESIAN_POINT ( 'NONE',  ( 4.000000000000003553, -8.999999999999992895, 0.3937499987709675020 ) ) ;
#16771 = CYLINDRICAL_SURFACE ( 'NONE', #18112, 27.10000000000000142 ) ;
#16772 = AXIS2_PLACEMENT_3D ( 'NONE', #11995, #9911, #14241 ) ;
#16773 = CARTESIAN_POINT ( 'NONE',  ( 29.99470236596032535, 8.217531866531109230, -6.500000000000000000 ) ) ;
#16774 = AXIS2_PLACEMENT_3D ( 'NONE', #7423, #7181, #3509 ) ;
#16775 = CARTESIAN_POINT ( 'NONE',  ( -3.959305671612554781E-15, -30.00000000000000355, 12.99999999999999289 ) ) ;
#16776 = CARTESIAN_POINT ( 'NONE',  ( 3.756430356250002323, -11.16877607737301226, 3.253124999385482941 ) ) ;
#16777 = DIRECTION ( 'NONE',  ( 0.000000000000000000, 0.000000000000000000, 1.000000000000000000 ) ) ;
#16778 = CARTESIAN_POINT ( 'NONE',  ( 3.752267015613588906E-15, -4.381197846482986158, 4.162500000000000533 ) ) ;
#16779 = DIRECTION ( 'NONE',  ( 0.000000000000000000, 0.000000000000000000, 1.000000000000000000 ) ) ;
#16780 = CARTESIAN_POINT ( 'NONE',  ( 0.4999838450259763700, 31.09598070739550124, -2.750000000000000000 ) ) ;
#16781 = CIRCLE ( 'NONE', #20093, 0.7500000000000001110 ) ;
#16782 = CARTESIAN_POINT ( 'NONE',  ( 3.735045420075836212E-15, -4.662447845253954171, 2.165624999385483029 ) ) ;
#16783 = CARTESIAN_POINT ( 'NONE',  ( 1.999999999999995781, -26.50000000000000355, 5.535898384862237620 ) ) ;
#16784 = DIRECTION ( 'NONE',  ( 0.5877852522924853496, 0.8090169943749385695, 0.000000000000000000 ) ) ;
#16785 = ORIENTED_EDGE ( 'NONE', *, *, #9525, .T. ) ;
#16786 = ORIENTED_EDGE ( 'NONE', *, *, #16353, .T. ) ;
#16787 = CARTESIAN_POINT ( 'NONE',  ( -3.756430356249994329, 29.11562499938548498, 11.16877607737301226 ) ) ;
#16788 = AXIS2_PLACEMENT_3D ( 'NONE', #4912, #14258, #391 ) ;
#16789 = ORIENTED_EDGE ( 'NONE', *, *, #25469, .T. ) ;
#16790 = PLANE ( 'NONE',  #17133 ) ;
#16791 = ORIENTED_EDGE ( 'NONE', *, *, #18426, .T. ) ;
#16792 = LINE ( 'NONE', #20704, #8374 ) ;
#16793 = EDGE_LOOP ( 'NONE', ( #935, #7095, #7203, #24654 ) ) ;
#16794 = DIRECTION ( 'NONE',  ( 1.000000000000000000, 0.000000000000000000, 0.000000000000000000 ) ) ;
#16795 = VECTOR ( 'NONE', #17257, 1000.000000000000000 ) ;
#16796 = AXIS2_PLACEMENT_3D ( 'NONE', #15335, #11267, #9569 ) ;
#16797 = EDGE_LOOP ( 'NONE', ( #25361, #21448, #7128, #20039 ) ) ;
#16798 = EDGE_CURVE ( 'NONE', #25452, #25113, #14338, .T. ) ;
#16799 = APPLICATION_CONTEXT ( 'automotive_design' ) ;
#16800 = CARTESIAN_POINT ( 'NONE',  ( 0.000000000000000000, 0.000000000000000000, -6.500000000000000000 ) ) ;
#16801 =( BOUNDED_CURVE ( )  B_SPLINE_CURVE ( 2, ( #12755, #8572, #18249, #12626, #6346, #10521, #16553 ),
 .UNSPECIFIED., .F., .F. ) 
 B_SPLINE_CURVE_WITH_KNOTS ( ( 3, 2, 2, 3 ),
 ( 0.3000000000000002109, 0.3166666666666668184, 0.3333333333333334814, 0.3500000000000000888 ),
 .UNSPECIFIED. ) 
 CURVE ( )  GEOMETRIC_REPRESENTATION_ITEM ( )  RATIONAL_B_SPLINE_CURVE ( ( 0.9999999999999982236, 0.8660254037844404840, 1.000000000000000000, 0.8660254037844387076, 1.000000000000000000, 0.8660254037844378194, 1.000000000000000888 ) ) 
 REPRESENTATION_ITEM ( '' )  );
#16802 = CARTESIAN_POINT ( 'NONE',  ( -3.999999999999996447, 25.67500000000000071, 8.999999999999992895 ) ) ;
#16803 = DIRECTION ( 'NONE',  ( 0.000000000000000000, 0.000000000000000000, -1.000000000000000000 ) ) ;
#16804 = AXIS2_PLACEMENT_3D ( 'NONE', #2291, #24634, #324 ) ;
#16805 = CARTESIAN_POINT ( 'NONE',  ( 27.09999999999999787, -0.5999999999999998668, 19.00000000000000000 ) ) ;
#16806 = CARTESIAN_POINT ( 'NONE',  ( -3.999999999999999112, 26.61250000000000426, 11.30940107675849404 ) ) ;
#16807 = CARTESIAN_POINT ( 'NONE',  ( 18.57260154916842154, 18.57260154916834693, 4.662447845253954171 ) ) ;
#16808 =( BOUNDED_CURVE ( )  B_SPLINE_CURVE ( 2, ( #24257, #24396, #2297, #16158, #12356, #2411, #11961, #10373, #18373, #4115, #20070, #10133, #17859, #22169, #12477, #19930, #18137, #8181, #4256, #2034, #329, #12230, #10003, #6472, #20197, #14458, #1914, #17998, #10254, #22420, #14580, #14967, #16552, #3071, #848, #20596, #20850, #24511, #4896, #7123, #6864, #2939, #22559, #14847, #10520, #22820, #18516, #11038, #10768, #24909, #16673, #720, #8964, #20994, #22698, #5030, #8686, #19017, #10904, #16939, #4641, #24640, #23083, #6728, #18637, #18901, #12624, #10642, #1101, #603, #6593, #20725, #9077, #14721, #2682, #983, #4780, #8829, #12753, #8570, #25033, #13011, #6985, #2803, #16818, #18758, #24781, #12873, #22946, #17060, #15109, #5169, #20450, #2550, #15491, #7255, #16106, #7374, #2108, #21861, #19272, #17203, #1373, #25174, #15235, #6031, #19878, #23321, #19403, #13399, #9348, #3455, #22, #15985, #9212, #1494, #23949, #159, #23460, #23200, #24070 ),
 .UNSPECIFIED., .F., .F. ) 
 B_SPLINE_CURVE_WITH_KNOTS ( ( 3, 2, 2, 2, 2, 2, 2, 2, 2, 2, 2, 2, 2, 2, 2, 2, 2, 2, 2, 2, 2, 2, 2, 2, 2, 2, 2, 2, 2, 2, 2, 2, 2, 2, 2, 2, 2, 2, 2, 2, 2, 2, 2, 2, 2, 2, 2, 2, 2, 2, 2, 2, 2, 2, 2, 2, 2, 2, 2, 2, 3 ),
 ( 0.000000000000000000, 0.01666666666666666644, 0.03333333333333333287, 0.05000000000000000278, 0.06666666666666666574, 0.08333333333333332871, 0.1000000000000000056, 0.1166666666666666685, 0.1333333333333333315, 0.1499999999999999944, 0.1666666666666666574, 0.1833333333333333204, 0.2000000000000000111, 0.2166666666666666741, 0.2333333333333333370, 0.2500000000000000000, 0.2666666666666666630, 0.2833333333333333259, 0.2999999999999999889, 0.3166666666666666519, 0.3333333333333333148, 0.3499999999999999778, 0.3666666666666666408, 0.3833333333333333592, 0.4000000000000000222, 0.4166666666666666852, 0.4333333333333333481, 0.4500000000000000111, 0.4666666666666666741, 0.4833333333333333370, 0.5000000000000000000, 0.5166666666666667185, 0.5333333333333333259, 0.5500000000000000444, 0.5666666666666666519, 0.5833333333333333703, 0.5999999999999999778, 0.6166666666666666963, 0.6333333333333333037, 0.6500000000000000222, 0.6666666666666666297, 0.6833333333333333481, 0.6999999999999999556, 0.7166666666666666741, 0.7333333333333332815, 0.7500000000000000000, 0.7666666666666667185, 0.7833333333333333259, 0.8000000000000000444, 0.8166666666666666519, 0.8333333333333333703, 0.8499999999999999778, 0.8666666666666666963, 0.8833333333333333037, 0.9000000000000000222, 0.9166666666666666297, 0.9333333333333333481, 0.9499999999999999556, 0.9666666666666666741, 0.9833333333333332815, 1.000000000000000000 ),
 .UNSPECIFIED. ) 
 CURVE ( )  GEOMETRIC_REPRESENTATION_ITEM ( )  RATIONAL_B_SPLINE_CURVE ( ( 1.000000000000000000, 0.8660254037844387076, 1.000000000000000000, 0.8660254037844387076, 1.000000000000000000, 0.8660254037844387076, 1.000000000000000000, 0.8660254037844387076, 1.000000000000000000, 0.8660254037844387076, 1.000000000000000000, 0.8660254037844387076, 1.000000000000000000, 0.8660254037844387076, 1.000000000000000000, 0.8660254037844387076, 1.000000000000000000, 0.8660254037844387076, 1.000000000000000000, 0.8660254037844387076, 1.000000000000000000, 0.8660254037844387076, 1.000000000000000000, 0.8660254037844387076, 1.000000000000000000, 0.8660254037844387076, 1.000000000000000000, 0.8660254037844387076, 1.000000000000000000, 0.8660254037844387076, 1.000000000000000000, 0.8660254037844387076, 1.000000000000000000, 0.8660254037844387076, 1.000000000000000000, 0.8660254037844387076, 1.000000000000000000, 0.8660254037844387076, 1.000000000000000000, 0.8660254037844387076, 1.000000000000000000, 0.8660254037844387076, 1.000000000000000000, 0.8660254037844387076, 1.000000000000000000, 0.8660254037844387076, 1.000000000000000000, 0.8660254037844387076, 1.000000000000000000, 0.8660254037844387076, 1.000000000000000000, 0.8660254037844387076, 1.000000000000000000, 0.8660254037844387076, 1.000000000000000000, 0.8660254037844387076, 1.000000000000000000, 0.8660254037844387076, 1.000000000000000000, 0.8660254037844387076, 1.000000000000000000, 0.8660254037844387076, 1.000000000000000000, 0.8660254037844387076, 1.000000000000000000, 0.8660254037844387076, 1.000000000000000000, 0.8660254037844387076, 1.000000000000000000, 0.8660254037844387076, 1.000000000000000000, 0.8660254037844387076, 1.000000000000000000, 0.8660254037844387076, 1.000000000000000000, 0.8660254037844387076, 1.000000000000000000, 0.8660254037844387076, 1.000000000000000000, 0.8660254037844387076, 1.000000000000000000, 0.8660254037844387076, 1.000000000000000000, 0.8660254037844387076, 1.000000000000000000, 0.8660254037844387076, 1.000000000000000000, 0.8660254037844387076, 1.000000000000000000, 0.8660254037844387076, 1.000000000000000000, 0.8660254037844387076, 1.000000000000000000, 0.8660254037844387076, 1.000000000000000000, 0.8660254037844387076, 1.000000000000000000, 0.8660254037844387076, 1.000000000000000000, 0.8660254037844387076, 1.000000000000000000, 0.8660254037844387076, 1.000000000000000000, 0.8660254037844387076, 1.000000000000000000, 0.8660254037844387076, 1.000000000000000000, 0.8660254037844387076, 1.000000000000000000, 0.8660254037844387076, 1.000000000000000000, 0.8660254037844387076, 1.000000000000000000, 0.8660254037844387076, 1.000000000000000000, 0.8660254037844387076, 1.000000000000000000, 0.8660254037844387076, 1.000000000000000000, 0.8660254037844387076, 1.000000000000000000 ) ) 
 REPRESENTATION_ITEM ( '' )  );
#16809 = AXIS2_PLACEMENT_3D ( 'NONE', #6816, #6425, #9031 ) ;
#16810 = CARTESIAN_POINT ( 'NONE',  ( 1.878215178125000939, 29.11562499938548498, 12.25316411605952283 ) ) ;
#16811 = AXIS2_PLACEMENT_3D ( 'NONE', #13226, #9690, #23417 ) ;
#16812 = VECTOR ( 'NONE', #12413, 1000.000000000000000 ) ;
#16813 = FACE_OUTER_BOUND ( 'NONE', #5698, .T. ) ;
#16814 = CARTESIAN_POINT ( 'NONE',  ( 18.96682627828696610, 17.45107675043485429, 12.99999999999999467 ) ) ;
#16815 = ORIENTED_EDGE ( 'NONE', *, *, #649, .F. ) ;
#16816 = DIRECTION ( 'NONE',  ( -0.000000000000000000, -0.000000000000000000, -1.000000000000000000 ) ) ;
#16817 = AXIS2_PLACEMENT_3D ( 'NONE', #18360, #11947, #24502 ) ;
#16818 = CARTESIAN_POINT ( 'NONE',  ( -3.756430356250003655, -28.29062499938548569, 8.999999999999992895 ) ) ;
#16819 = DIRECTION ( 'NONE',  ( 0.000000000000000000, 0.000000000000000000, 1.000000000000000000 ) ) ;
#16820 = CARTESIAN_POINT ( 'NONE',  ( -3.756430356249995661, 26.34062499938548285, 6.831223922626973533 ) ) ;
#16821 = CARTESIAN_POINT ( 'NONE',  ( 1.952783444825901382, 29.93753283725207481, 12.50294890599017172 ) ) ;
#16822 = VERTEX_POINT ( 'NONE', #18248 ) ;
#16823 = VERTEX_POINT ( 'NONE', #9875 ) ;
#16824 = CARTESIAN_POINT ( 'NONE',  ( -3.918623196469518177, 38.49999999999999289, 4.456389954662586028 ) ) ;
#16825 = CIRCLE ( 'NONE', #5540, 0.5000000000000003331 ) ;
#16826 = EDGE_CURVE ( 'NONE', #5382, #20504, #8443, .T. ) ;
#16827 = DIRECTION ( 'NONE',  ( 1.000000000000000000, 0.000000000000000000, 0.000000000000000000 ) ) ;
#16828 = ORIENTED_EDGE ( 'NONE', *, *, #21161, .F. ) ;
#16829 = CARTESIAN_POINT ( 'NONE',  ( -2.672651547586948120E-15, -27.39062499938548356, 13.33755215474603162 ) ) ;
#16830 = CARTESIAN_POINT ( 'NONE',  ( -28.14012133169306296, 13.24173596767408867, 1.000000000000000000 ) ) ;
#16831 = CARTESIAN_POINT ( 'NONE',  ( 1.878215178125003382, 25.66562499938548214, 5.746835883940462963 ) ) ;
#16832 = AXIS2_PLACEMENT_3D ( 'NONE', #16037, #6203, #12090 ) ;
#16833 = EDGE_CURVE ( 'NONE', #24266, #6036, #15648, .T. ) ;
#16834 = CARTESIAN_POINT ( 'NONE',  ( -1.859271017917182139E-15, 26.46249999999999858, 4.999999999999991118 ) ) ;
#16835 = CARTESIAN_POINT ( 'NONE',  ( 0.000000000000000000, 25.78750000000000497, 13.61880215351699874 ) ) ;
#16836 = ADVANCED_FACE ( 'NONE', ( #8304 ), #13944, .F. ) ;
#16837 = PLANE ( 'NONE',  #2590 ) ;
#16838 = VECTOR ( 'NONE', #25398, 1000.000000000000000 ) ;
#16839 = LINE ( 'NONE', #622, #12111 ) ;
#16840 = ADVANCED_FACE ( 'NONE', ( #4377 ), #21912, .F. ) ;
#16841 = DIRECTION ( 'NONE',  ( 0.000000000000000000, 0.000000000000000000, 1.000000000000000000 ) ) ;
#16842 = DIRECTION ( 'NONE',  ( -0.000000000000000000, -1.000000000000000000, -0.000000000000000000 ) ) ;
#16843 = AXIS2_PLACEMENT_3D ( 'NONE', #18234, #317, #18358 ) ;
#16844 = CARTESIAN_POINT ( 'NONE',  ( 3.756430356250003655, 25.59062499938548285, 8.999999999999992895 ) ) ;
#16845 = CARTESIAN_POINT ( 'NONE',  ( 3.834746474454188013E-15, 25.56250000000000000, 4.999999999999992006 ) ) ;
#16846 = CARTESIAN_POINT ( 'NONE',  ( 20.79777820164935775, 15.14092395215691234, 11.30940107675849760 ) ) ;
#16847 = CARTESIAN_POINT ( 'NONE',  ( 18.41350252340144422, 18.41350252340138383, 13.33755215474602984 ) ) ;
#16848 = LINE ( 'NONE', #12781, #12210 ) ;
#16849 = DIRECTION ( 'NONE',  ( -0.000000000000000000, -0.000000000000000000, -1.000000000000000000 ) ) ;
#16850 = CARTESIAN_POINT ( 'NONE',  ( 1.878215178125004048, 27.91562499938548569, 5.746835883940462963 ) ) ;
#16851 = CARTESIAN_POINT ( 'NONE',  ( 28.34936733434205536, 12.78762572734047254, -2.750000000000000000 ) ) ;
#16852 = CARTESIAN_POINT ( 'NONE',  ( 18.49305203628493643, 18.49305203628486183, 4.662447845253954171 ) ) ;
#16853 = CARTESIAN_POINT ( 'NONE',  ( 3.959305671612554781E-15, 35.50000000000000711, 12.99999999999999289 ) ) ;
#16854 = ORIENTED_EDGE ( 'NONE', *, *, #466, .F. ) ;
#16855 = CARTESIAN_POINT ( 'NONE',  ( 3.469446951953614189E-15, 35.50000000000000711, 8.999999999999992895 ) ) ;
#16856 = CARTESIAN_POINT ( 'NONE',  ( -1.999999999999998224, 27.49374999877096926, 12.46410161513774639 ) ) ;
#16857 = CARTESIAN_POINT ( 'NONE',  ( -1.878215178125004048, -29.26562499938548356, 5.746835883940462963 ) ) ;
#16859 = ORIENTED_EDGE ( 'NONE', *, *, #2432, .T. ) ;
#16858 = CARTESIAN_POINT ( 'NONE',  ( -1.999999999999998224, 25.30000000000000426, 12.46410161513774639 ) ) ;
#16860 = CARTESIAN_POINT ( 'NONE',  ( -29.99470236596021167, 8.217531866531519569, -2.750000000000000000 ) ) ;
#16861 = AXIS2_PLACEMENT_3D ( 'NONE', #19638, #23186, #15474 ) ;
#16862 = ORIENTED_EDGE ( 'NONE', *, *, #14086, .F. ) ;
#16863 = CARTESIAN_POINT ( 'NONE',  ( -2.672651547586948120E-15, -26.37812499938548427, 13.33755215474602984 ) ) ;
#16864 = VERTEX_POINT ( 'NONE', #20322 ) ;
#16865 = ORIENTED_EDGE ( 'NONE', *, *, #17402, .F. ) ;
#16866 = FACE_OUTER_BOUND ( 'NONE', #4474, .T. ) ;
#16867 = CARTESIAN_POINT ( 'NONE',  ( -3.756430356249996105, 27.69062499938548427, 6.831223922626973533 ) ) ;
#16868 = AXIS2_PLACEMENT_3D ( 'NONE', #14388, #14504, #24443 ) ;
#16869 = CARTESIAN_POINT ( 'NONE',  ( -30.91344420362550593, -3.401318489840770010, -6.500000000000000000 ) ) ;
#16870 = CARTESIAN_POINT ( 'NONE',  ( -1.878215178124995832, -5.746835883940462963, 2.203124999385484895 ) ) ;
#16871 = SURFACE_STYLE_FILL_AREA ( #24445 ) ;
#16872 = EDGE_CURVE ( 'NONE', #16293, #1927, #16808, .T. ) ;
#16873 = DIRECTION ( 'NONE',  ( 0.000000000000000000, 0.000000000000000000, 1.000000000000000000 ) ) ;
#16874 = CARTESIAN_POINT ( 'NONE',  ( -1.878215178124998497, 28.59062499938548285, 12.25316411605951927 ) ) ;
#16875 = EDGE_CURVE ( 'NONE', #18617, #20603, #5284, .T. ) ;
#16876 = FACE_OUTER_BOUND ( 'NONE', #15936, .T. ) ;
#16877 = CARTESIAN_POINT ( 'NONE',  ( -10.94867358849309547, 28.91604871112477326, -6.500000000000000000 ) ) ;
#16878 = CARTESIAN_POINT ( 'NONE',  ( 1.878215178125000939, 28.21562499938548640, 12.25316411605952283 ) ) ;
#16879 = CARTESIAN_POINT ( 'NONE',  ( 16.87775498257738960, 22.53460923206970179, 8.999999999999992895 ) ) ;
#16880 = CARTESIAN_POINT ( 'NONE',  ( -30.45149776762733751, -6.317933499823126908, -6.500000000000000000 ) ) ;
#16881 = FACE_OUTER_BOUND ( 'NONE', #4939, .T. ) ;
#16882 = DIRECTION ( 'NONE',  ( 1.000000000000000000, 0.000000000000000000, 0.000000000000000000 ) ) ;
#16883 = CARTESIAN_POINT ( 'NONE',  ( -3.756430356250002323, -26.56562499938548427, 11.16877607737301226 ) ) ;
#16884 = CARTESIAN_POINT ( 'NONE',  ( 3.756430356250003655, 26.15312499938548640, 8.999999999999992895 ) ) ;
#16885 = CARTESIAN_POINT ( 'NONE',  ( 25.99307600111999150, 0.6000000000000000888, 20.00001200000000168 ) ) ;
#16886 = AXIS2_PLACEMENT_3D ( 'NONE', #12770, #2698, #16309 ) ;
#16887 = FACE_OUTER_BOUND ( 'NONE', #16303, .T. ) ;
#16888 = CARTESIAN_POINT ( 'NONE',  ( 3.180741987853693331, -29.83126030492351788, 11.43940974718624837 ) ) ;
#16889 = VERTEX_POINT ( 'NONE', #21111 ) ;
#16890 = DIRECTION ( 'NONE',  ( 0.000000000000000000, 0.000000000000000000, 1.000000000000000000 ) ) ;
#16892 = ORIENTED_EDGE ( 'NONE', *, *, #4735, .F. ) ;
#16891 = CARTESIAN_POINT ( 'NONE',  ( 10.98232076577222038, 29.09636799667079288, -6.500000000000000000 ) ) ;
#16893 = ORIENTED_EDGE ( 'NONE', *, *, #5528, .T. ) ;
#16894 = EDGE_LOOP ( 'NONE', ( #14021, #16110, #20938, #20640 ) ) ;
#16895 = EDGE_LOOP ( 'NONE', ( #21229, #10916, #23334, #23892 ) ) ;
#16896 = VERTEX_POINT ( 'NONE', #17330 ) ;
#16897 = CARTESIAN_POINT ( 'NONE',  ( -2.000000000000003997, -27.77500000000000213, 5.535898384862238508 ) ) ;
#16898 = STYLED_ITEM ( 'NONE', ( #25468 ), #4445 ) ;
#16899 = ORIENTED_EDGE ( 'NONE', *, *, #11563, .F. ) ;
#16900 = CYLINDRICAL_SURFACE ( 'NONE', #24461, 4.000000000000000000 ) ;
#16901 = CARTESIAN_POINT ( 'NONE',  ( -1.878215178124998497, 28.70312499938548356, 12.25316411605951927 ) ) ;
#16902 = EDGE_CURVE ( 'NONE', #19632, #14980, #10367, .T. ) ;
#16903 = CARTESIAN_POINT ( 'NONE',  ( -1.878215178124995832, -5.746835883940462963, 0.2906249993854838065 ) ) ;
#16904 = FILL_AREA_STYLE ('',( #946 ) ) ;
#16905 = CARTESIAN_POINT ( 'NONE',  ( -4.000000000000003553, -25.43124999877097281, 6.690598923241489970 ) ) ;
#16906 = CARTESIAN_POINT ( 'NONE',  ( 3.469446951953614189E-15, 34.00000000000000000, 4.999999999999992006 ) ) ;
#16907 = EDGE_CURVE ( 'NONE', #15184, #22241, #17931, .T. ) ;
#16908 = CARTESIAN_POINT ( 'NONE',  ( -11.52193136556784658, -23.36965697125209118, 20.00001200000000168 ) ) ;
#16909 = CARTESIAN_POINT ( 'NONE',  ( 3.756430356250004099, -6.831223922626973533, 3.328124999385480898 ) ) ;
#16910 = CARTESIAN_POINT ( 'NONE',  ( 30.00000000000000355, 3.673940397442059967E-15, 0.000000000000000000 ) ) ;
#16911 = FACE_OUTER_BOUND ( 'NONE', #17210, .T. ) ;
#16912 = CYLINDRICAL_SURFACE ( 'NONE', #8011, 0.5000000000000004441 ) ;
#16913 = CARTESIAN_POINT ( 'NONE',  ( -3.999999999999996447, -8.999999999999992895, 2.868749998770965703 ) ) ;
#16914 = CARTESIAN_POINT ( 'NONE',  ( 3.756430356250002323, -11.16877607737301403, 3.815624999385481164 ) ) ;
#16915 = DIRECTION ( 'NONE',  ( -0.7071067811865487940, -0.7071067811865463515, -0.000000000000000000 ) ) ;
#16916 = CARTESIAN_POINT ( 'NONE',  ( -3.834746474454188013E-15, -26.01249999999999574, 4.999999999999992006 ) ) ;
#16917 = ORIENTED_EDGE ( 'NONE', *, *, #7830, .T. ) ;
#16918 = ORIENTED_EDGE ( 'NONE', *, *, #3594, .T. ) ;
#16919 = ORIENTED_EDGE ( 'NONE', *, *, #12919, .T. ) ;
#16920 = DIRECTION ( 'NONE',  ( 1.000000000000000000, 0.000000000000000000, 0.000000000000000000 ) ) ;
#16921 = VERTEX_POINT ( 'NONE', #3316 ) ;
#16922 = CARTESIAN_POINT ( 'NONE',  ( 3.756430356249995661, -26.34062499938548285, 6.831223922626973533 ) ) ;
#16923 = ORIENTED_EDGE ( 'NONE', *, *, #14254, .T. ) ;
#16924 = CARTESIAN_POINT ( 'NONE',  ( -1.999999999999996669, 27.94374999877097565, 12.46410161513774639 ) ) ;
#16925 = ORIENTED_EDGE ( 'NONE', *, *, #22050, .F. ) ;
#16926 = DIRECTION ( 'NONE',  ( 0.000000000000000000, -1.000000000000000000, 0.000000000000000000 ) ) ;
#16927 = CARTESIAN_POINT ( 'NONE',  ( -3.756430356249997882, 28.55312499938548498, 11.16877607737301226 ) ) ;
#16928 = CARTESIAN_POINT ( 'NONE',  ( -26.75313774936430633, -14.98253926456308172, 1.000000000000000000 ) ) ;
#16929 = CARTESIAN_POINT ( 'NONE',  ( 17.43018215624843847, 20.25860928099455904, 12.46410161513774639 ) ) ;
#16930 = CARTESIAN_POINT ( 'NONE',  ( 22.39552511608559371, 17.08313036016677700, 11.16877607737301226 ) ) ;
#16931 = ADVANCED_FACE ( 'NONE', ( #20007 ), #9467, .F. ) ;
#16932 = CARTESIAN_POINT ( 'NONE',  ( -1.071796769724487230, 28.28259618943233988, 4.999999999999992006 ) ) ;
#16933 = CARTESIAN_POINT ( 'NONE',  ( 3.735045420075836212E-15, 29.30312499938548498, 4.662447845253954171 ) ) ;
#16934 = EDGE_CURVE ( 'NONE', #6185, #17868, #17444, .T. ) ;
#16935 = CARTESIAN_POINT ( 'NONE',  ( 16.65886629145492748, 21.97126104737360563, 11.16877607737301048 ) ) ;
#16936 = CARTESIAN_POINT ( 'NONE',  ( -1.952785157361201618, 31.03863125411927371, 1.000000000000000000 ) ) ;
#16937 = VERTEX_POINT ( 'NONE', #14015 ) ;
#16938 = CARTESIAN_POINT ( 'NONE',  ( -2.003086131649545506E-15, 27.08124999877097139, 13.61880215351699874 ) ) ;
#16939 = CARTESIAN_POINT ( 'NONE',  ( -3.756430356250002323, -27.35312499938547859, 11.16877607737301403 ) ) ;
#16940 = EDGE_CURVE ( 'NONE', #15884, #15503, #19138, .T. ) ;
#16941 = CARTESIAN_POINT ( 'NONE',  ( -3.999999999999997335, 27.06250000000000000, 11.30940107675849404 ) ) ;
#16942 = CARTESIAN_POINT ( 'NONE',  ( 2.000000000000000888, 29.36874999877096926, 12.46410161513774817 ) ) ;
#16943 = CARTESIAN_POINT ( 'NONE',  ( 0.000000000000000000, 0.000000000000000000, 16.00000000000000000 ) ) ;
#16945 = ORIENTED_EDGE ( 'NONE', *, *, #22768, .F. ) ;
#16944 = CARTESIAN_POINT ( 'NONE',  ( 0.000000000000000000, 28.74062499938548854, 13.33755215474603162 ) ) ;
#16946 = ORIENTED_EDGE ( 'NONE', *, *, #4828, .T. ) ;
#16947 =( BOUNDED_SURFACE ( )  B_SPLINE_SURFACE ( 1, 2, ( 
 ( #25859, #4019, #23906, #2202, #11985, #19577, #3899, #9657, #18029, #1818, #19959, #10162, #1680, #9782, #17762, #25731, #13838, #11870, #19837, #1938, #2322, #12651, #14364, #8332, #16457, #4528, #24289, #18274, #22324, #4286, #6374, #501, #24419, #10280, #16575, #24672, #12509, #20483, #6760, #12258, #24148, #20226, #745, #237, #8471, #4671, #8208, #361, #22199, #10797, #22448, #14745, #2581, #16320, #22589, #16181, #10403, #14481, #22724, #6496, #4804, #6238, #10545, #18544, #14228, #12381, #6619, #626, #4405, #12779, #8593, #14608, #24534, #20346, #2443, #18403, #20623, #2706, #2829, #10667, #18658, #8714, #16701, #20750, #25318, #19300, #20880, #7281, #3480, #24931, #14871, #1258, #25061, #5309, #7150, #1399, #12904, #7397, #21020, #7010, #9372, #11320, #3344, #1125, #22846, #21401, #5062, #13287, #14996, #4919, #17353, #15377, #23349, #24809, #13041, #5438, #23225, #21263, #13429, #18789, #2968 ),
 ( #10935, #16964, #19042, #17089, #18926, #9242, #876, #23109, #5191, #8859, #1010, #16846, #8987, #6888, #22975, #9100, #3097, #11064, #15140, #13169, #21138, #3211, #11181, #19165, #17231, #15258, #25203, #21641, #25703, #17992, #9752, #82, #22029, #11706, #21781, #9486, #23611, #17855, #5818, #19426, #8053, #19809, #25827, #1785, #21520, #9620, #17599, #1911, #7662, #14063, #25577, #15645, #9871, #5574, #1644, #16036, #11957, #13553, #7911, #11453, #5691, #7523, #15898, #13670, #17732, #3601, #1517, #23998, #23871, #6077, #23488, #3724, #7783, #25439, #11571, #17467, #19684, #15764, #15520, #3865, #23730, #2029, #13802, #19541, #11838, #5956, #13941, #21908, #3990, #19926, #9998, #18132, #16427, #717, #14455, #24392, #2168, #12619, #20317, #8566, #325, #10249, #18513, #4636, #6340, #14576, #18244, #20593, #4497, #2292, #8300, #16668, #16287, #8439, #24253, #20448, #16549, #206, #10369, #468, #14716 ) ),
 .UNSPECIFIED., .F., .F., .F. ) 
 B_SPLINE_SURFACE_WITH_KNOTS ( ( 2, 2 ),
 ( 3, 2, 2, 2, 2, 2, 2, 2, 2, 2, 2, 2, 2, 2, 2, 2, 2, 2, 2, 2, 2, 2, 2, 2, 2, 2, 2, 2, 2, 2, 2, 2, 2, 2, 2, 2, 2, 2, 2, 2, 2, 2, 2, 2, 2, 2, 2, 2, 2, 2, 2, 2, 2, 2, 2, 2, 2, 2, 2, 2, 3 ),
 ( 0.000000000000000000, 1.000000000000000000 ),
 ( 0.000000000000000000, 0.01666666666666666644, 0.03333333333333333287, 0.05000000000000000278, 0.06666666666666666574, 0.08333333333333332871, 0.1000000000000000056, 0.1166666666666666685, 0.1333333333333333315, 0.1499999999999999944, 0.1666666666666666574, 0.1833333333333333204, 0.2000000000000000111, 0.2166666666666666741, 0.2333333333333333370, 0.2500000000000000000, 0.2666666666666666630, 0.2833333333333333259, 0.2999999999999999889, 0.3166666666666666519, 0.3333333333333333148, 0.3499999999999999778, 0.3666666666666666408, 0.3833333333333333592, 0.4000000000000000222, 0.4166666666666666852, 0.4333333333333333481, 0.4500000000000000111, 0.4666666666666666741, 0.4833333333333333370, 0.5000000000000000000, 0.5166666666666667185, 0.5333333333333333259, 0.5500000000000000444, 0.5666666666666666519, 0.5833333333333333703, 0.5999999999999999778, 0.6166666666666666963, 0.6333333333333333037, 0.6500000000000000222, 0.6666666666666666297, 0.6833333333333333481, 0.6999999999999999556, 0.7166666666666666741, 0.7333333333333332815, 0.7500000000000000000, 0.7666666666666667185, 0.7833333333333333259, 0.8000000000000000444, 0.8166666666666666519, 0.8333333333333333703, 0.8499999999999999778, 0.8666666666666666963, 0.8833333333333333037, 0.9000000000000000222, 0.9166666666666666297, 0.9333333333333333481, 0.9499999999999999556, 0.9666666666666666741, 0.9833333333333332815, 1.000000000000000000 ),
 .UNSPECIFIED. ) 
 GEOMETRIC_REPRESENTATION_ITEM ( )  RATIONAL_B_SPLINE_SURFACE ( (
 ( 1.000000000000000000, 0.8660254037844387076, 1.000000000000000000, 0.8660254037844387076, 1.000000000000000000, 0.8660254037844387076, 1.000000000000000000, 0.8660254037844387076, 1.000000000000000000, 0.8660254037844387076, 1.000000000000000000, 0.8660254037844387076, 1.000000000000000000, 0.8660254037844387076, 1.000000000000000000, 0.8660254037844387076, 1.000000000000000000, 0.8660254037844387076, 1.000000000000000000, 0.8660254037844387076, 1.000000000000000000, 0.8660254037844387076, 1.000000000000000000, 0.8660254037844387076, 1.000000000000000000, 0.8660254037844387076, 1.000000000000000000, 0.8660254037844387076, 1.000000000000000000, 0.8660254037844387076, 1.000000000000000000, 0.8660254037844387076, 1.000000000000000000, 0.8660254037844387076, 1.000000000000000000, 0.8660254037844387076, 1.000000000000000000, 0.8660254037844387076, 1.000000000000000000, 0.8660254037844387076, 1.000000000000000000, 0.8660254037844387076, 1.000000000000000000, 0.8660254037844387076, 1.000000000000000000, 0.8660254037844387076, 1.000000000000000000, 0.8660254037844387076, 1.000000000000000000, 0.8660254037844387076, 1.000000000000000000, 0.8660254037844387076, 1.000000000000000000, 0.8660254037844387076, 1.000000000000000000, 0.8660254037844387076, 1.000000000000000000, 0.8660254037844387076, 1.000000000000000000, 0.8660254037844387076, 1.000000000000000000, 0.8660254037844387076, 1.000000000000000000, 0.8660254037844387076, 1.000000000000000000, 0.8660254037844387076, 1.000000000000000000, 0.8660254037844387076, 1.000000000000000000, 0.8660254037844387076, 1.000000000000000000, 0.8660254037844387076, 1.000000000000000000, 0.8660254037844387076, 1.000000000000000000, 0.8660254037844387076, 1.000000000000000000, 0.8660254037844387076, 1.000000000000000000, 0.8660254037844387076, 1.000000000000000000, 0.8660254037844387076, 1.000000000000000000, 0.8660254037844387076, 1.000000000000000000, 0.8660254037844387076, 1.000000000000000000, 0.8660254037844387076, 1.000000000000000000, 0.8660254037844387076, 1.000000000000000000, 0.8660254037844387076, 1.000000000000000000, 0.8660254037844387076, 1.000000000000000000, 0.8660254037844387076, 1.000000000000000000, 0.8660254037844387076, 1.000000000000000000, 0.8660254037844387076, 1.000000000000000000, 0.8660254037844387076, 1.000000000000000000, 0.8660254037844387076, 1.000000000000000000, 0.8660254037844387076, 1.000000000000000000, 0.8660254037844387076, 1.000000000000000000, 0.8660254037844387076, 1.000000000000000000, 0.8660254037844387076, 1.000000000000000000, 0.8660254037844387076, 1.000000000000000000, 0.8660254037844387076, 1.000000000000000000, 0.8660254037844387076, 1.000000000000000000, 0.8660254037844387076, 1.000000000000000000),
 ( 1.000000000000000000, 0.8660254037844387076, 1.000000000000000000, 0.8660254037844387076, 1.000000000000000000, 0.8660254037844387076, 1.000000000000000000, 0.8660254037844387076, 1.000000000000000000, 0.8660254037844387076, 1.000000000000000000, 0.8660254037844387076, 1.000000000000000000, 0.8660254037844387076, 1.000000000000000000, 0.8660254037844387076, 1.000000000000000000, 0.8660254037844387076, 1.000000000000000000, 0.8660254037844387076, 1.000000000000000000, 0.8660254037844387076, 1.000000000000000000, 0.8660254037844387076, 1.000000000000000000, 0.8660254037844387076, 1.000000000000000000, 0.8660254037844387076, 1.000000000000000000, 0.8660254037844387076, 1.000000000000000000, 0.8660254037844387076, 1.000000000000000000, 0.8660254037844387076, 1.000000000000000000, 0.8660254037844387076, 1.000000000000000000, 0.8660254037844387076, 1.000000000000000000, 0.8660254037844387076, 1.000000000000000000, 0.8660254037844387076, 1.000000000000000000, 0.8660254037844387076, 1.000000000000000000, 0.8660254037844387076, 1.000000000000000000, 0.8660254037844387076, 1.000000000000000000, 0.8660254037844387076, 1.000000000000000000, 0.8660254037844387076, 1.000000000000000000, 0.8660254037844387076, 1.000000000000000000, 0.8660254037844387076, 1.000000000000000000, 0.8660254037844387076, 1.000000000000000000, 0.8660254037844387076, 1.000000000000000000, 0.8660254037844387076, 1.000000000000000000, 0.8660254037844387076, 1.000000000000000000, 0.8660254037844387076, 1.000000000000000000, 0.8660254037844387076, 1.000000000000000000, 0.8660254037844387076, 1.000000000000000000, 0.8660254037844387076, 1.000000000000000000, 0.8660254037844387076, 1.000000000000000000, 0.8660254037844387076, 1.000000000000000000, 0.8660254037844387076, 1.000000000000000000, 0.8660254037844387076, 1.000000000000000000, 0.8660254037844387076, 1.000000000000000000, 0.8660254037844387076, 1.000000000000000000, 0.8660254037844387076, 1.000000000000000000, 0.8660254037844387076, 1.000000000000000000, 0.8660254037844387076, 1.000000000000000000, 0.8660254037844387076, 1.000000000000000000, 0.8660254037844387076, 1.000000000000000000, 0.8660254037844387076, 1.000000000000000000, 0.8660254037844387076, 1.000000000000000000, 0.8660254037844387076, 1.000000000000000000, 0.8660254037844387076, 1.000000000000000000, 0.8660254037844387076, 1.000000000000000000, 0.8660254037844387076, 1.000000000000000000, 0.8660254037844387076, 1.000000000000000000, 0.8660254037844387076, 1.000000000000000000, 0.8660254037844387076, 1.000000000000000000, 0.8660254037844387076, 1.000000000000000000, 0.8660254037844387076, 1.000000000000000000, 0.8660254037844387076, 1.000000000000000000, 0.8660254037844387076, 1.000000000000000000) ) ) 
 REPRESENTATION_ITEM ( '' )  SURFACE ( )  );
#16948 = CARTESIAN_POINT ( 'NONE',  ( -1.057460391440397258E-14, 29.55624999877096926, 4.999999999999992006 ) ) ;
#16949 = CARTESIAN_POINT ( 'NONE',  ( 1.071796769724494558, 26.38615380933864074, 4.999999999999992895 ) ) ;
#16950 = ORIENTED_EDGE ( 'NONE', *, *, #2915, .F. ) ;
#16951 = CARTESIAN_POINT ( 'NONE',  ( -1.878215178125004048, -29.37812499938548783, 5.746835883940462963 ) ) ;
#16952 = CARTESIAN_POINT ( 'NONE',  ( 23.69483382651587888, 18.38243907059705151, 8.999999999999992895 ) ) ;
#16953 =( BOUNDED_CURVE ( )  B_SPLINE_CURVE ( 2, ( #19693, #25448, #7534, #13563, #1268, #3219, #15266, #21409, #5317 ),
 .UNSPECIFIED., .F., .F. ) 
 B_SPLINE_CURVE_WITH_KNOTS ( ( 3, 2, 2, 2, 3 ),
 ( 0.2750000000000000222, 0.2833333333333333259, 0.2999999999999999889, 0.3166666666666666519, 0.3250000000000000111 ),
 .UNSPECIFIED. ) 
 CURVE ( )  GEOMETRIC_REPRESENTATION_ITEM ( )  RATIONAL_B_SPLINE_CURVE ( ( 0.9330127018922194093, 0.9330127018922196314, 1.000000000000000000, 0.8660254037844387076, 1.000000000000000000, 0.8660254037844387076, 1.000000000000000000, 0.9330127018922191873, 0.9330127018922194093 ) ) 
 REPRESENTATION_ITEM ( '' )  );
#16954 = DIRECTION ( 'NONE',  ( -0.9921147013144768767, 0.1253332335643120576, 0.000000000000000000 ) ) ;
#16955 = AXIS2_PLACEMENT_3D ( 'NONE', #9032, #15055, #23034 ) ;
#16956 = DIRECTION ( 'NONE',  ( -0.000000000000000000, -1.000000000000000000, -0.000000000000000000 ) ) ;
#16957 = CARTESIAN_POINT ( 'NONE',  ( 4.000000000000002665, 25.48750000000000426, 6.690598923241489970 ) ) ;
#16958 = CARTESIAN_POINT ( 'NONE',  ( 10.98232076577222038, 29.09636799667079288, -2.750000000000000000 ) ) ;
#16959 = DIRECTION ( 'NONE',  ( 1.000000000000000000, 0.000000000000000000, 0.000000000000000000 ) ) ;
#16960 = DIRECTION ( 'NONE',  ( 1.000000000000000000, 0.000000000000000000, 0.000000000000000000 ) ) ;
#16961 = EDGE_CURVE ( 'NONE', #8582, #125, #22130, .T. ) ;
#16962 = CARTESIAN_POINT ( 'NONE',  ( 3.735045420075836212E-15, 27.95312499938548001, 4.662447845253954171 ) ) ;
#16963 = CARTESIAN_POINT ( 'NONE',  ( 21.73911410323489690, 16.08225985374244615, 8.999999999999992895 ) ) ;
#16964 = CARTESIAN_POINT ( 'NONE',  ( 20.53261315870440740, 14.87575890921195665, 6.690598923241489970 ) ) ;
#16965 = CARTESIAN_POINT ( 'NONE',  ( 20.08631576820957321, 17.43011839025013288, 12.25316411605952283 ) ) ;
#16966 = CARTESIAN_POINT ( 'NONE',  ( 0.000000000000000000, 0.000000000000000000, 19.50000000000000000 ) ) ;
#16967 = CARTESIAN_POINT ( 'NONE',  ( -3.756430356249997882, 27.65312499938548640, 11.16877607737301226 ) ) ;
#16969 = EDGE_CURVE ( 'NONE', #1309, #12702, #14574, .T. ) ;
#16968 = CARTESIAN_POINT ( 'NONE',  ( 1.394453263437886604E-15, 28.88124999877097210, 12.99999999999999289 ) ) ;
#16970 = CARTESIAN_POINT ( 'NONE',  ( 16.87099832581089132, 22.18339308172956237, 8.999999999999992895 ) ) ;
#16971 = CARTESIAN_POINT ( 'NONE',  ( 20.74032577480890183, 20.74032577480883077, 12.99999999999999289 ) ) ;
#16972 = EDGE_CURVE ( 'NONE', #17764, #4035, #7925, .T. ) ;
#16973 = ORIENTED_EDGE ( 'NONE', *, *, #14358, .F. ) ;
#16974 = CARTESIAN_POINT ( 'NONE',  ( -21.28941499438192864, 22.67092431280617859, 1.000000000000000000 ) ) ;
#16975 = CARTESIAN_POINT ( 'NONE',  ( 3.752267015613588906E-15, 28.20624999877096784, 4.381197846482986158 ) ) ;
#16976 = CARTESIAN_POINT ( 'NONE',  ( 1.999999999999998224, -25.30000000000000426, 12.46410161513774639 ) ) ;
#16978 = ORIENTED_EDGE ( 'NONE', *, *, #2480, .T. ) ;
#16977 = DIRECTION ( 'NONE',  ( -0.000000000000000000, -0.000000000000000000, -1.000000000000000000 ) ) ;
#16979 = CARTESIAN_POINT ( 'NONE',  ( 3.735045420075836212E-15, 26.71562499938548285, 4.662447845253954171 ) ) ;
#16980 = ORIENTED_EDGE ( 'NONE', *, *, #13131, .F. ) ;
#16981 = CARTESIAN_POINT ( 'NONE',  ( 1.878215178124998497, -27.69062499938548427, 12.25316411605951927 ) ) ;
#16982 = ORIENTED_EDGE ( 'NONE', *, *, #4922, .T. ) ;
#16983 = ADVANCED_FACE ( 'NONE', ( #14522 ), #24579, .F. ) ;
#16984 = ORIENTED_EDGE ( 'NONE', *, *, #23440, .F. ) ;
#16985 = CARTESIAN_POINT ( 'NONE',  ( 20.83968866226292249, 21.58177178539264318, 5.025996973432255821 ) ) ;
#16986 = CARTESIAN_POINT ( 'NONE',  ( -3.756430356249998326, 27.24062499938548854, 6.831223922626973533 ) ) ;
#16987 = FACE_OUTER_BOUND ( 'NONE', #6937, .T. ) ;
#16988 = CARTESIAN_POINT ( 'NONE',  ( 2.000000000000000888, 28.91874999877096997, 12.46410161513774817 ) ) ;
#16989 =( NAMED_UNIT ( * ) PLANE_ANGLE_UNIT ( ) SI_UNIT ( $, .RADIAN. ) );
#16990 = EDGE_CURVE ( 'NONE', #20797, #2274, #10712, .T. ) ;
#16991 = DIRECTION ( 'NONE',  ( 1.000000000000000000, 0.000000000000000000, 0.000000000000000000 ) ) ;
#16992 = CARTESIAN_POINT ( 'NONE',  ( -1.878215178124995832, 28.44062499938548427, 5.746835883940462963 ) ) ;
#16993 = DIRECTION ( 'NONE',  ( 1.000000000000000000, 0.000000000000000000, 0.000000000000000000 ) ) ;
#16994 = DIRECTION ( 'NONE',  ( -0.7071067811865487940, -0.7071067811865463515, 0.000000000000000000 ) ) ;
#16995 = PRODUCT_DEFINITION_CONTEXT ( 'detailed design', #16799, 'design' ) ;
#16996 = CARTESIAN_POINT ( 'NONE',  ( -1.878215178124995832, 27.54062499938548214, 5.746835883940462963 ) ) ;
#16997 = CARTESIAN_POINT ( 'NONE',  ( -9.610428525061097460, -29.57785765677920509, 1.000000000000000000 ) ) ;
#16998 = CARTESIAN_POINT ( 'NONE',  ( 3.959305671612554781E-15, 30.00000000000000355, 12.99999999999999289 ) ) ;
#16999 = DIRECTION ( 'NONE',  ( 0.000000000000000000, 1.000000000000000000, 0.000000000000000000 ) ) ;
#17000 = DIRECTION ( 'NONE',  ( 1.000000000000000000, 0.000000000000000000, 0.000000000000000000 ) ) ;
#17001 = CARTESIAN_POINT ( 'NONE',  ( 3.756430356249995661, -25.89062499938548356, 6.831223922626973533 ) ) ;
#17002 = CARTESIAN_POINT ( 'NONE',  ( 2.672651547586948120E-15, 25.59062499938548640, 13.33755215474602984 ) ) ;
#17003 = DIRECTION ( 'NONE',  ( -0.2486898871648449971, 0.9685831611286336296, 0.000000000000000000 ) ) ;
#17004 = LINE ( 'NONE', #23021, #9577 ) ;
#17005 = CARTESIAN_POINT ( 'NONE',  ( -19.82388608118395013, 23.96296185032730364, -6.500000000000000000 ) ) ;
#17006 = VERTEX_POINT ( 'NONE', #24337 ) ;
#17007 = LINE ( 'NONE', #1441, #10433 ) ;
#17009 = ORIENTED_EDGE ( 'NONE', *, *, #19948, .T. ) ;
#17008 = CARTESIAN_POINT ( 'NONE',  ( 0.000000000000000000, 0.000000000000000000, 18.19999999999999929 ) ) ;
#17010 = EDGE_CURVE ( 'NONE', #12604, #1927, #548, .T. ) ;
#17011 = ORIENTED_EDGE ( 'NONE', *, *, #19677, .F. ) ;
#17012 = ORIENTED_EDGE ( 'NONE', *, *, #23952, .F. ) ;
#17013 = VERTEX_POINT ( 'NONE', #2489 ) ;
#17014 = EDGE_CURVE ( 'NONE', #21660, #22219, #14657, .T. ) ;
#17015 = ORIENTED_EDGE ( 'NONE', *, *, #21739, .T. ) ;
#17016 = DIRECTION ( 'NONE',  ( 1.000000000000000000, 0.000000000000000000, 0.000000000000000000 ) ) ;
#17018 = EDGE_CURVE ( 'NONE', #7884, #19632, #8378, .T. ) ;
#17017 = CARTESIAN_POINT ( 'NONE',  ( -3.110308778861272216, 31.50000000000000000, 14.13088484572967296 ) ) ;
#17019 = ORIENTED_EDGE ( 'NONE', *, *, #19586, .F. ) ;
#17020 = CARTESIAN_POINT ( 'NONE',  ( 3.756430356250003211, 29.34062499938548640, 6.831223922626973533 ) ) ;
#17021 = CARTESIAN_POINT ( 'NONE',  ( 3.756430356250004099, -6.831223922626973533, 1.078124999385482452 ) ) ;
#17022 = DIRECTION ( 'NONE',  ( 0.9980267284282724471, 0.06279051952930156388, 0.000000000000000000 ) ) ;
#17023 = CARTESIAN_POINT ( 'NONE',  ( 20.40224034548861809, 20.40224034548853638, 4.662447845253954171 ) ) ;
#17024 = CARTESIAN_POINT ( 'NONE',  ( 2.672651547586948120E-15, 26.94062499938548783, 13.33755215474602984 ) ) ;
#17025 = CARTESIAN_POINT ( 'NONE',  ( -25.16843286583315376, -6.741346781237213648, 20.00001200000000168 ) ) ;
#17026 = CARTESIAN_POINT ( 'NONE',  ( 3.756430356250002323, -11.16877607737301226, 4.153124999385482852 ) ) ;
#17027 = CARTESIAN_POINT ( 'NONE',  ( 19.82388608118429119, 23.96296185032701587, -6.500000000000000000 ) ) ;
#17028 = DIRECTION ( 'NONE',  ( -0.000000000000000000, -0.000000000000000000, 1.000000000000000000 ) ) ;
#17029 = DIRECTION ( 'NONE',  ( 0.000000000000000000, 0.000000000000000000, 1.000000000000000000 ) ) ;
#17030 = CARTESIAN_POINT ( 'NONE',  ( -8.366719580627318441E-15, 29.55624999877097281, 4.999999999999992006 ) ) ;
#17031 = CARTESIAN_POINT ( 'NONE',  ( -3.756430356249997438, -11.16877607737301048, 4.565624999385485161 ) ) ;
#17032 = FACE_OUTER_BOUND ( 'NONE', #19001, .T. ) ;
#17033 = CARTESIAN_POINT ( 'NONE',  ( -1.071796769724492338, -25.80759618943233491, 12.99999999999999467 ) ) ;
#17034 = ORIENTED_EDGE ( 'NONE', *, *, #7074, .F. ) ;
#17035 = VERTEX_POINT ( 'NONE', #18455 ) ;
#17036 = ORIENTED_EDGE ( 'NONE', *, *, #1628, .F. ) ;
#17037 = FACE_OUTER_BOUND ( 'NONE', #15236, .T. ) ;
#17038 = ORIENTED_EDGE ( 'NONE', *, *, #20462, .F. ) ;
#17039 = DIRECTION ( 'NONE',  ( -0.000000000000000000, -0.000000000000000000, 1.000000000000000000 ) ) ;
#17040 = EDGE_CURVE ( 'NONE', #3427, #20732, #22639, .T. ) ;
#17041 = ORIENTED_EDGE ( 'NONE', *, *, #15059, .F. ) ;
#17042 = EDGE_CURVE ( 'NONE', #14631, #23924, #4578, .T. ) ;
#17043 = ORIENTED_EDGE ( 'NONE', *, *, #19273, .F. ) ;
#17044 = LINE ( 'NONE', #13127, #4309 ) ;
#17045 = CARTESIAN_POINT ( 'NONE',  ( -3.999999999999996447, 25.22500000000000142, 8.999999999999992895 ) ) ;
#17046 = ADVANCED_FACE ( 'NONE', ( #24198 ), #12302, .T. ) ;
#17047 = CARTESIAN_POINT ( 'NONE',  ( 1.071796769724481901, -27.56740381056766864, 12.99999999999999645 ) ) ;
#17048 = AXIS2_PLACEMENT_3D ( 'NONE', #15590, #23560, #4053 ) ;
#17049 = FACE_OUTER_BOUND ( 'NONE', #24885, .T. ) ;
#17050 = DIRECTION ( 'NONE',  ( 0.000000000000000000, 0.000000000000000000, 1.000000000000000000 ) ) ;
#17051 = CARTESIAN_POINT ( 'NONE',  ( 21.14924941424430571, 15.83685465832548900, 8.999999999999992895 ) ) ;
#17052 = DIRECTION ( 'NONE',  ( -0.000000000000000000, -1.000000000000000000, -0.000000000000000000 ) ) ;
#17053 =( BOUNDED_CURVE ( )  B_SPLINE_CURVE ( 2, ( #23876, #21786, #5821, #25321, #17858, #11456, #13806, #5577, #7527 ),
 .UNSPECIFIED., .F., .F. ) 
 B_SPLINE_CURVE_WITH_KNOTS ( ( 3, 2, 2, 2, 3 ),
 ( 0.6750000000000000444, 0.6833333333333333481, 0.6999999999999999556, 0.7166666666666666741, 0.7249999999999999778 ),
 .UNSPECIFIED. ) 
 CURVE ( )  GEOMETRIC_REPRESENTATION_ITEM ( )  RATIONAL_B_SPLINE_CURVE ( ( 0.9330127018922194093, 0.9330127018922198534, 1.000000000000000000, 0.8660254037844387076, 1.000000000000000000, 0.8660254037844387076, 1.000000000000000000, 0.9330127018922194093, 0.9330127018922194093 ) ) 
 REPRESENTATION_ITEM ( '' )  );
#17054 = VECTOR ( 'NONE', #18442, 1000.000000000000114 ) ;
#17055 = CARTESIAN_POINT ( 'NONE',  ( 4.000000000000003553, 25.90000000000000213, 8.999999999999992895 ) ) ;
#17056 = CARTESIAN_POINT ( 'NONE',  ( 17.29526239452281899, 22.60765715044149715, 11.16877607737301048 ) ) ;
#17057 = CARTESIAN_POINT ( 'NONE',  ( -3.469446951953614189E-15, -30.00000000000000355, 4.999999999999992006 ) ) ;
#17058 = EDGE_LOOP ( 'NONE', ( #8161, #8769, #7612, #23 ) ) ;
#17059 = CARTESIAN_POINT ( 'NONE',  ( 0.000000000000000000, 28.43124999877097636, 13.61880215351699874 ) ) ;
#17060 = CARTESIAN_POINT ( 'NONE',  ( 3.756430356249996105, -28.47812499938548569, 6.831223922626973533 ) ) ;
#17061 = AXIS2_PLACEMENT_3D ( 'NONE', #10584, #18579, #2103 ) ;
#17062 = DIRECTION ( 'NONE',  ( 1.000000000000000000, 0.000000000000000000, 0.000000000000000000 ) ) ;
#17063 = CARTESIAN_POINT ( 'NONE',  ( -3.756430356249997882, 27.31562499938548427, 11.16877607737301226 ) ) ;
#17064 = CARTESIAN_POINT ( 'NONE',  ( 2.205873879792267900, 29.91968208057595646, 12.34935938736416894 ) ) ;
#17066 = EDGE_LOOP ( 'NONE', ( #22006, #8689, #7646, #22568 ) ) ;
#17065 = CARTESIAN_POINT ( 'NONE',  ( -3.756430356249996994, -8.999999999999992895, 0.3656249993854825409 ) ) ;
#17067 = ORIENTED_EDGE ( 'NONE', *, *, #20094, .F. ) ;
#17068 = DIRECTION ( 'NONE',  ( -0.000000000000000000, -0.000000000000000000, 1.000000000000000000 ) ) ;
#17070 = EDGE_CURVE ( 'NONE', #8796, #2564, #2365, .T. ) ;
#17069 = AXIS2_PLACEMENT_3D ( 'NONE', #3554, #5764, #13750 ) ;
#17071 = CARTESIAN_POINT ( 'NONE',  ( 2.000000000000000888, 26.21874999877096712, 12.46410161513774817 ) ) ;
#17072 = VECTOR ( 'NONE', #13077, 1000.000000000000000 ) ;
#17073 = ORIENTED_EDGE ( 'NONE', *, *, #3970, .T. ) ;
#17074 = DIRECTION ( 'NONE',  ( -0.3090169943749382919, 0.9510565162951566398, 0.000000000000000000 ) ) ;
#17075 = FACE_OUTER_BOUND ( 'NONE', #25180, .T. ) ;
#17076 = FACE_OUTER_BOUND ( 'NONE', #15954, .T. ) ;
#17077 = CARTESIAN_POINT ( 'NONE',  ( 22.41528496361359046, 16.75843071412113972, 8.999999999999992895 ) ) ;
#17078 = CARTESIAN_POINT ( 'NONE',  ( 3.756430356250003211, 29.19062499938548072, 8.999999999999992895 ) ) ;
#17079 = ADVANCED_FACE ( 'NONE', ( #283 ), #6417, .F. ) ;
#17080 = AXIS2_PLACEMENT_3D ( 'NONE', #25295, #15351, #13147 ) ;
#17081 = DIRECTION ( 'NONE',  ( 0.000000000000000000, 0.000000000000000000, 1.000000000000000000 ) ) ;
#17082 = AXIS2_PLACEMENT_3D ( 'NONE', #25858, #8331, #7946 ) ;
#17083 = APPLICATION_PROTOCOL_DEFINITION ( 'draft international standard', 'automotive_design', 1998, #16799 ) ;
#17084 = DIRECTION ( 'NONE',  ( 1.000000000000000000, 0.000000000000000000, 0.000000000000000000 ) ) ;
#17085 = DIRECTION ( 'NONE',  ( 0.000000000000000000, 0.000000000000000000, -1.000000000000000000 ) ) ;
#17086 = CARTESIAN_POINT ( 'NONE',  ( -3.756430356249996105, 26.22812499938548214, 6.831223922626973533 ) ) ;
#17087 = AXIS2_PLACEMENT_3D ( 'NONE', #17388, #25485, #5347 ) ;
#17088 = CARTESIAN_POINT ( 'NONE',  ( -1.071796769724487675, 26.87634618820331411, 4.999999999999992895 ) ) ;
#17089 = CARTESIAN_POINT ( 'NONE',  ( 17.75721904254720940, 17.75721904254714545, 4.381197846482986158 ) ) ;
#17090 = CARTESIAN_POINT ( 'NONE',  ( 21.12273290994980712, 15.81033815403099752, 11.16877607737301226 ) ) ;
#17091 = DIRECTION ( 'NONE',  ( 0.000000000000000000, 0.000000000000000000, -1.000000000000000000 ) ) ;
#17092 = CARTESIAN_POINT ( 'NONE',  ( 3.756430356250004099, 27.42812499938548143, 6.831223922626973533 ) ) ;
#17093 = CARTESIAN_POINT ( 'NONE',  ( 0.000000000000000000, 0.000000000000000000, 1.000000000000000000 ) ) ;
#17094 = CARTESIAN_POINT ( 'NONE',  ( 20.11283227250407180, 17.45663489454462436, 5.746835883940462963 ) ) ;
#17095 = CARTESIAN_POINT ( 'NONE',  ( 23.64830241243857500, 17.99144816294611715, 8.999999999999992895 ) ) ;
#17096 = ORIENTED_EDGE ( 'NONE', *, *, #3561, .T. ) ;
#17097 = CARTESIAN_POINT ( 'NONE',  ( -3.999999999999997335, 25.65624999877097068, 11.30940107675849404 ) ) ;
#17098 = CARTESIAN_POINT ( 'NONE',  ( -1.999999999999995781, 28.69374999877096855, 5.535898384862237620 ) ) ;
#17099 = CARTESIAN_POINT ( 'NONE',  ( -4.000000000000003553, -25.44999999999999929, 8.999999999999992895 ) ) ;
#17101 = ORIENTED_EDGE ( 'NONE', *, *, #12482, .F. ) ;
#17100 = CARTESIAN_POINT ( 'NONE',  ( 23.96296185032695192, -19.82388608118436935, -6.500000000000000000 ) ) ;
#17102 = CARTESIAN_POINT ( 'NONE',  ( 2.672651547586948120E-15, 26.49062499938548498, 13.33755215474603162 ) ) ;
#17103 =( BOUNDED_CURVE ( )  B_SPLINE_CURVE ( 2, ( #156, #20004, #13746, #20141, #21722, #21858, #1859, #5897, #23810 ),
 .UNSPECIFIED., .F., .F. ) 
 B_SPLINE_CURVE_WITH_KNOTS ( ( 3, 2, 2, 2, 3 ),
 ( 0.1250000000000000000, 0.1333333333333333315, 0.1499999999999999944, 0.1666666666666666574, 0.1749999999999999889 ),
 .UNSPECIFIED. ) 
 CURVE ( )  GEOMETRIC_REPRESENTATION_ITEM ( )  RATIONAL_B_SPLINE_CURVE ( ( 0.9330127018922194093, 0.9330127018922194093, 1.000000000000000000, 0.8660254037844387076, 1.000000000000000000, 0.8660254037844387076, 1.000000000000000000, 0.9330127018922194093, 0.9330127018922194093 ) ) 
 REPRESENTATION_ITEM ( '' )  );
#17104 = AXIS2_PLACEMENT_3D ( 'NONE', #5867, #13851, #19972 ) ;
#17105 = ORIENTED_EDGE ( 'NONE', *, *, #25465, .T. ) ;
#17106 = CARTESIAN_POINT ( 'NONE',  ( -3.735045420075836212E-15, -29.30312499938548498, 4.662447845253954171 ) ) ;
#17107 = VERTEX_POINT ( 'NONE', #22365 ) ;
#17108 = ORIENTED_EDGE ( 'NONE', *, *, #1646, .T. ) ;
#17109 = CARTESIAN_POINT ( 'NONE',  ( 18.19544668900821094, 23.85216383888419855, 8.737301635141733414 ) ) ;
#17110 = CARTESIAN_POINT ( 'NONE',  ( 3.756430356250000546, 28.36562499938549564, 11.16877607737301226 ) ) ;
#17111 = VECTOR ( 'NONE', #593, 1000.000000000000000 ) ;
#17112 = AXIS2_PLACEMENT_3D ( 'NONE', #15494, #23708, #5793 ) ;
#17113 = ADVANCED_FACE ( 'NONE', ( #20145 ), #6288, .F. ) ;
#17114 = CARTESIAN_POINT ( 'NONE',  ( 1.878215178125004048, -5.746835883940462963, 1.115624999385483207 ) ) ;
#17115 = CIRCLE ( 'NONE', #11670, 0.5000000000000001110 ) ;
#17116 = CARTESIAN_POINT ( 'NONE',  ( 1.878215178125004048, -5.746835883940462963, 4.378124999385484273 ) ) ;
#17117 =( NAMED_UNIT ( * ) PLANE_ANGLE_UNIT ( ) SI_UNIT ( $, .RADIAN. ) );
#17118 = ADVANCED_FACE ( 'NONE', ( #8251 ), #12421, .T. ) ;
#17119 = CARTESIAN_POINT ( 'NONE',  ( -1.071796769724495668, -27.15759618943233633, 12.99999999999999112 ) ) ;
#17120 = AXIS2_PLACEMENT_3D ( 'NONE', #1253, #22969, #9236 ) ;
#17121 = CARTESIAN_POINT ( 'NONE',  ( 4.000000000000007105, 29.08750000000000568, 6.690598923241489970 ) ) ;
#17122 = AXIS2_PLACEMENT_3D ( 'NONE', #6900, #25213, #4933 ) ;
#17123 = DIRECTION ( 'NONE',  ( 0.000000000000000000, 0.000000000000000000, -1.000000000000000000 ) ) ;
#17124 = CARTESIAN_POINT ( 'NONE',  ( 3.756430356250003211, 28.77812499938548285, 6.831223922626973533 ) ) ;
#17125 = DIRECTION ( 'NONE',  ( 1.000000000000000000, 0.000000000000000000, 0.000000000000000000 ) ) ;
#17126 = CARTESIAN_POINT ( 'NONE',  ( -25.75859848311282363, -16.66421332384654974, -6.500000000000000000 ) ) ;
#17127 = CARTESIAN_POINT ( 'NONE',  ( 3.959305671612554781E-15, 40.00000000000000000, 12.99999999999999289 ) ) ;
#17128 = CARTESIAN_POINT ( 'NONE',  ( -2.000000000000000888, -27.56874999877096855, 12.46410161513774817 ) ) ;
#17129 = CARTESIAN_POINT ( 'NONE',  ( 3.756430356249995661, -28.59062499938548640, 6.831223922626973533 ) ) ;
#17130 = DIRECTION ( 'NONE',  ( 1.000000000000000000, 0.000000000000000000, 0.000000000000000000 ) ) ;
#17131 = CIRCLE ( 'NONE', #5010, 31.10000000000000142 ) ;
#17132 = CARTESIAN_POINT ( 'NONE',  ( 2.000000000000000888, 27.56874999877096855, 12.46410161513774817 ) ) ;
#17134 = CARTESIAN_POINT ( 'NONE',  ( -3.999999999999996447, -8.999999999999992895, 4.275000000000001243 ) ) ;
#17133 = AXIS2_PLACEMENT_3D ( 'NONE', #22920, #6842, #14825 ) ;
#17135 = CYLINDRICAL_SURFACE ( 'NONE', #10550, 0.5000000000000004441 ) ;
#17136 = APPLICATION_CONTEXT ( 'automotive_design' ) ;
#17137 = ORIENTED_EDGE ( 'NONE', *, *, #17280, .T. ) ;
#17138 = DIRECTION ( 'NONE',  ( 0.000000000000000000, -0.000000000000000000, 1.000000000000000000 ) ) ;
#17140 = ORIENTED_EDGE ( 'NONE', *, *, #2052, .T. ) ;
#17139 = DIRECTION ( 'NONE',  ( -0.8443279255020205154, -0.5358267949789882190, 0.000000000000000000 ) ) ;
#17141 = ORIENTED_EDGE ( 'NONE', *, *, #3927, .T. ) ;
#17142 = CIRCLE ( 'NONE', #20453, 31.10000000000000142 ) ;
#17143 = ORIENTED_EDGE ( 'NONE', *, *, #22508, .F. ) ;
#17144 = ORIENTED_EDGE ( 'NONE', *, *, #20699, .F. ) ;
#17145 = VERTEX_POINT ( 'NONE', #22104 ) ;
#17146 = DIRECTION ( 'NONE',  ( -0.000000000000000000, 0.000000000000000000, 1.000000000000000000 ) ) ;
#17147 = VECTOR ( 'NONE', #8788, 999.9999999999998863 ) ;
#17148 = DIRECTION ( 'NONE',  ( -1.000000000000000000, 0.000000000000000000, 0.000000000000000000 ) ) ;
#17149 = CIRCLE ( 'NONE', #1264, 31.10000000000000142 ) ;
#17150 = EDGE_CURVE ( 'NONE', #15986, #20673, #2246, .T. ) ;
#17151 = CARTESIAN_POINT ( 'NONE',  ( 3.756430356250003655, -8.999999999999992895, 4.753124999385485161 ) ) ;
#17152 = CARTESIAN_POINT ( 'NONE',  ( 4.000000000000003553, -6.690598923241489970, 1.331249998770967169 ) ) ;
#17153 = CARTESIAN_POINT ( 'NONE',  ( 22.97888821056449515, 17.66649345464567489, 8.999999999999992895 ) ) ;
#17154 = ADVANCED_FACE ( 'NONE', ( #14279 ), #22243, .F. ) ;
#17155 = FACE_OUTER_BOUND ( 'NONE', #14824, .T. ) ;
#17156 = CARTESIAN_POINT ( 'NONE',  ( 26.49999999999999645, -0.5000000000000000000, 19.50000000000000000 ) ) ;
#17157 = CARTESIAN_POINT ( 'NONE',  ( 4.000000000000001776, 28.50624999877096855, 11.30940107675849760 ) ) ;
#17158 = AXIS2_PLACEMENT_3D ( 'NONE', #10101, #17960, #48 ) ;
#17159 = CARTESIAN_POINT ( 'NONE',  ( 2.000000000000003997, -5.535898384862238508, 0.07499999999999867883 ) ) ;
#17160 = DIRECTION ( 'NONE',  ( 0.000000000000000000, 0.000000000000000000, 1.000000000000000000 ) ) ;
#17162 = EDGE_CURVE ( 'NONE', #23030, #4688, #23367, .T. ) ;
#17161 = CARTESIAN_POINT ( 'NONE',  ( 0.000000000000000000, 0.000000000000000000, -6.500000000000000000 ) ) ;
#17163 = CARTESIAN_POINT ( 'NONE',  ( -27.64012133169306296, 13.24173596767408867, -6.500000000000000000 ) ) ;
#17164 = CARTESIAN_POINT ( 'NONE',  ( -1.999999999999994893, 29.59374999877097068, 5.535898384862237620 ) ) ;
#17165 = AXIS2_PLACEMENT_3D ( 'NONE', #9516, #9399, #13582 ) ;
#17166 = CARTESIAN_POINT ( 'NONE',  ( 4.000000000000003553, -6.690598923241489970, 0.4312499987709677018 ) ) ;
#17167 = AXIS2_PLACEMENT_3D ( 'NONE', #17822, #8015, #25789 ) ;
#17168 = CARTESIAN_POINT ( 'NONE',  ( 1.071796769724488563, -26.66740381056766651, 12.99999999999999289 ) ) ;
#17169 = CARTESIAN_POINT ( 'NONE',  ( -3.999999999999980904, -6.690598923241480200, 4.181249998770965703 ) ) ;
#17170 = VERTEX_POINT ( 'NONE', #7321 ) ;
#17171 = DIRECTION ( 'NONE',  ( 0.000000000000000000, 0.000000000000000000, 1.000000000000000000 ) ) ;
#17172 = AXIS2_PLACEMENT_3D ( 'NONE', #24791, #10915, #10652 ) ;
#17173 = ORIENTED_EDGE ( 'NONE', *, *, #25260, .F. ) ;
#17174 = AXIS2_PLACEMENT_3D ( 'NONE', #18185, #24323, #20130 ) ;
#17175 = VERTEX_POINT ( 'NONE', #22886 ) ;
#17176 = CARTESIAN_POINT ( 'NONE',  ( 4.000000000000003553, -8.999999999999992895, 4.893749998770967835 ) ) ;
#17177 = ORIENTED_EDGE ( 'NONE', *, *, #25793, .T. ) ;
#17178 = CARTESIAN_POINT ( 'NONE',  ( -3.756430356250002323, -25.66562499938548569, 11.16877607737301226 ) ) ;
#17179 = ORIENTED_EDGE ( 'NONE', *, *, #25820, .F. ) ;
#17180 = CARTESIAN_POINT ( 'NONE',  ( -3.999999999999997335, 28.86250000000000071, 11.30940107675849404 ) ) ;
#17181 = ORIENTED_EDGE ( 'NONE', *, *, #3339, .T. ) ;
#17182 = CARTESIAN_POINT ( 'NONE',  ( 3.999999999999997335, -29.31250000000000000, 11.30940107675849404 ) ) ;
#17183 = CARTESIAN_POINT ( 'NONE',  ( 3.752267015613588906E-15, 27.36250000000000071, 4.381197846482986158 ) ) ;
#17184 = CARTESIAN_POINT ( 'NONE',  ( -13.24173596767398742, -28.14012133169310559, 1.000000000000000000 ) ) ;
#17185 = VECTOR ( 'NONE', #11129, 1000.000000000000000 ) ;
#17186 = AXIS2_PLACEMENT_3D ( 'NONE', #3239, #9130, #17123 ) ;
#17187 = DIRECTION ( 'NONE',  ( 0.000000000000000000, -0.000000000000000000, 1.000000000000000000 ) ) ;
#17188 = PRODUCT_RELATED_PRODUCT_CATEGORY ( 'part', '', ( #4426 ) ) ;
#17189 = CARTESIAN_POINT ( 'NONE',  ( -26.00000000000000355, -1.592040838891558504E-15, 20.00000599999999906 ) ) ;
#17190 = CARTESIAN_POINT ( 'NONE',  ( 16.28763523133199342, 21.60002998725066448, 6.831223922626973533 ) ) ;
#17191 = AXIS2_PLACEMENT_3D ( 'NONE', #19715, #6233, #2197 ) ;
#17192 = CARTESIAN_POINT ( 'NONE',  ( -3.999999999999997335, 28.41250000000000142, 11.30940107675849404 ) ) ;
#17193 = ADVANCED_FACE ( 'NONE', ( #15301 ), #4970, .F. ) ;
#17194 = CARTESIAN_POINT ( 'NONE',  ( -3.999999999999996447, 25.67500000000000071, 8.999999999999992895 ) ) ;
#17195 = EDGE_CURVE ( 'NONE', #21040, #14500, #9587, .T. ) ;
#17196 = CARTESIAN_POINT ( 'NONE',  ( 16.92403133439988139, 22.23642609031855599, 6.831223922626973533 ) ) ;
#17197 = CARTESIAN_POINT ( 'NONE',  ( 3.959305671612554781E-15, 30.00000000000000355, 12.99999999999999289 ) ) ;
#17198 = AXIS2_PLACEMENT_3D ( 'NONE', #20054, #12079, #17848 ) ;
#17199 = VERTEX_POINT ( 'NONE', #5351 ) ;
#17200 = VERTEX_POINT ( 'NONE', #16891 ) ;
#17201 = CARTESIAN_POINT ( 'NONE',  ( 4.000000000000003553, 26.74374999877097281, 8.999999999999992895 ) ) ;
#17202 = CIRCLE ( 'NONE', #10498, 0.4999999999999996114 ) ;
#17203 = CARTESIAN_POINT ( 'NONE',  ( 3.756430356249996105, -28.92812499938548498, 6.831223922626973533 ) ) ;
#17204 = AXIS2_PLACEMENT_3D ( 'NONE', #16394, #2385, #10338 ) ;
#17205 = DIRECTION ( 'NONE',  ( 1.000000000000000000, 0.000000000000000000, 0.000000000000000000 ) ) ;
#17206 = CARTESIAN_POINT ( 'NONE',  ( -3.756430356249996994, 26.82812499938548711, 8.999999999999992895 ) ) ;
#17207 = VECTOR ( 'NONE', #10209, 1000.000000000000000 ) ;
#17208 = LINE ( 'NONE', #11161, #7521 ) ;
#17209 = VERTEX_POINT ( 'NONE', #21063 ) ;
#17210 = EDGE_LOOP ( 'NONE', ( #6544, #6779, #22110, #13629 ) ) ;
#17211 = DIRECTION ( 'NONE',  ( -0.4817536741017063306, 0.8763066800438685799, 0.000000000000000000 ) ) ;
#17212 = AXIS2_PLACEMENT_3D ( 'NONE', #6923, #22878, #24092 ) ;
#17213 = DIRECTION ( 'NONE',  ( 1.000000000000000000, 0.000000000000000000, 0.000000000000000000 ) ) ;
#17214 = ORIENTED_EDGE ( 'NONE', *, *, #17014, .T. ) ;
#17215 = CARTESIAN_POINT ( 'NONE',  ( -1.878215178125000939, -29.22812499938548569, 12.25316411605952283 ) ) ;
#17216 = DIRECTION ( 'NONE',  ( -0.000000000000000000, -0.000000000000000000, 1.000000000000000000 ) ) ;
#17217 = CARTESIAN_POINT ( 'NONE',  ( -3.756430356249996549, 26.22812499938548569, 6.831223922626973533 ) ) ;
#17218 = CIRCLE ( 'NONE', #12612, 0.5000000000000004441 ) ;
#17219 = CARTESIAN_POINT ( 'NONE',  ( 6.009258394948636914E-15, 29.30312499938549564, 4.662447845253954171 ) ) ;
#17220 = CIRCLE ( 'NONE', #23459, 6.000000000000000000 ) ;
#17221 = CIRCLE ( 'NONE', #23077, 31.10000000000000142 ) ;
#17222 = ADVANCED_FACE ( 'NONE', ( #24855 ), #19211, .T. ) ;
#17223 = FACE_OUTER_BOUND ( 'NONE', #12727, .T. ) ;
#17224 = SHAPE_DEFINITION_REPRESENTATION ( #14673, #20528 ) ;
#17225 = AXIS2_PLACEMENT_3D ( 'NONE', #12004, #18053, #5494 ) ;
#17226 = AXIS2_PLACEMENT_3D ( 'NONE', #14748, #20752, #20625 ) ;
#17227 = EDGE_CURVE ( 'NONE', #20939, #25359, #21277, .T. ) ;
#17228 = CARTESIAN_POINT ( 'NONE',  ( 3.469446951953614189E-15, 30.00000000000000355, 8.999999999999992895 ) ) ;
#17229 = CARTESIAN_POINT ( 'NONE',  ( 3.756430356250003211, 26.97812499938547859, 6.831223922626973533 ) ) ;
#17230 = LINE ( 'NONE', #1643, #6612 ) ;
#17231 = CARTESIAN_POINT ( 'NONE',  ( 21.14249275747780032, 15.48563850798535491, 8.999999999999992895 ) ) ;
#17232 = CARTESIAN_POINT ( 'NONE',  ( 21.17576591853879719, 15.86337116261998048, 6.831223922626973533 ) ) ;
#17233 = LINE ( 'NONE', #1260, #18429 ) ;
#17234 = CARTESIAN_POINT ( 'NONE',  ( 3.756430356250003655, 28.29062499938548569, 8.999999999999992895 ) ) ;
#17235 = CARTESIAN_POINT ( 'NONE',  ( 23.23716070179032656, 18.97547230650486938, 6.356741067357148722 ) ) ;
#17236 = VECTOR ( 'NONE', #17146, 1000.000000000000000 ) ;
#17237 = CARTESIAN_POINT ( 'NONE',  ( 21.27955846146187113, 18.62336108350243080, 12.25316411605952283 ) ) ;
#17238 = CARTESIAN_POINT ( 'NONE',  ( 17.67766952966372429, 17.67766952966365679, 8.999999999999992895 ) ) ;
#17239 = ORIENTED_EDGE ( 'NONE', *, *, #8199, .F. ) ;
#17240 = FACE_OUTER_BOUND ( 'NONE', #25733, .T. ) ;
#17241 = CARTESIAN_POINT ( 'NONE',  ( -3.756430356249995661, 26.34062499938548285, 6.831223922626973533 ) ) ;
#17242 = CARTESIAN_POINT ( 'NONE',  ( -1.878215178125000939, -27.76562499938548356, 12.25316411605952283 ) ) ;
#17244 = ORIENTED_EDGE ( 'NONE', *, *, #16311, .T. ) ;
#17243 = DIRECTION ( 'NONE',  ( 1.000000000000000000, 0.000000000000000000, 0.000000000000000000 ) ) ;
#17245 = CARTESIAN_POINT ( 'NONE',  ( -3.756430356249997438, 26.41562499938548569, 11.16877607737301048 ) ) ;
#17246 = VECTOR ( 'NONE', #9051, 1000.000000000000000 ) ;
#17247 = EDGE_CURVE ( 'NONE', #19150, #22740, #9990, .T. ) ;
#17248 = ORIENTED_EDGE ( 'NONE', *, *, #8819, .T. ) ;
#17249 = CARTESIAN_POINT ( 'NONE',  ( 3.756430356249997882, -27.65312499938548640, 11.16877607737301226 ) ) ;
#17250 = EDGE_LOOP ( 'NONE', ( #7230, #5653, #6218, #11081 ) ) ;
#17251 = ORIENTED_EDGE ( 'NONE', *, *, #9867, .F. ) ;
#17252 = DIRECTION ( 'NONE',  ( 0.000000000000000000, 0.000000000000000000, 1.000000000000000000 ) ) ;
#17253 = CARTESIAN_POINT ( 'NONE',  ( -1.878215178124998275, 28.25312499938548783, 12.25316411605951927 ) ) ;
#17254 = CARTESIAN_POINT ( 'NONE',  ( -1.878215178124998497, -12.25316411605951927, 1.340624999385482630 ) ) ;
#17255 = AXIS2_PLACEMENT_3D ( 'NONE', #2344, #24555, #10300 ) ;
#17256 = DIRECTION ( 'NONE',  ( -0.000000000000000000, 0.000000000000000000, -1.000000000000000000 ) ) ;
#17257 = DIRECTION ( 'NONE',  ( -0.000000000000000000, -0.000000000000000000, 1.000000000000000000 ) ) ;
#17258 = CIRCLE ( 'NONE', #25188, 31.10000000000000142 ) ;
#17259 = CARTESIAN_POINT ( 'NONE',  ( 21.21320343559646915, 21.21320343559638744, 8.999999999999992895 ) ) ;
#17260 = CARTESIAN_POINT ( 'NONE',  ( 0.000000000000000000, 0.000000000000000000, 1.000000000000000000 ) ) ;
#17261 = UNCERTAINTY_MEASURE_WITH_UNIT (LENGTH_MEASURE( 1.000000000000000082E-05 ), #12116, 'distance_accuracy_value', 'NONE');
#17262 = CARTESIAN_POINT ( 'NONE',  ( -1.952783444825901382, -29.93753283725207481, 12.50294890599017172 ) ) ;
#17263 = CARTESIAN_POINT ( 'NONE',  ( -1.999999999999998224, 27.04374999877096641, 12.46410161513774639 ) ) ;
#17264 = DIRECTION ( 'NONE',  ( -0.000000000000000000, -0.000000000000000000, 1.000000000000000000 ) ) ;
#17265 = DIRECTION ( 'NONE',  ( 0.000000000000000000, 0.000000000000000000, 1.000000000000000000 ) ) ;
#17266 = DIRECTION ( 'NONE',  ( -1.000000000000000000, 0.000000000000000000, 0.000000000000000000 ) ) ;
#17267 = CARTESIAN_POINT ( 'NONE',  ( -3.735045420075836212E-15, -28.51562499938549067, 4.662447845253954171 ) ) ;
#17268 =( BOUNDED_CURVE ( )  B_SPLINE_CURVE ( 2, ( #8150, #7878, #24091, #25675, #20167, #6174, #12053 ),
 .UNSPECIFIED., .F., .F. ) 
 B_SPLINE_CURVE_WITH_KNOTS ( ( 3, 2, 2, 3 ),
 ( 0.7500000000000000000, 0.7666666666666667185, 0.7833333333333332149, 0.7999999999999999334 ),
 .UNSPECIFIED. ) 
 CURVE ( )  GEOMETRIC_REPRESENTATION_ITEM ( )  RATIONAL_B_SPLINE_CURVE ( ( 1.000000000000000000, 0.8660254037844387076, 1.000000000000000000, 0.8660254037844387076, 1.000000000000000000, 0.8660254037844395958, 0.9999999999999991118 ) ) 
 REPRESENTATION_ITEM ( '' )  );
#17269 = DIRECTION ( 'NONE',  ( 1.000000000000000000, 0.000000000000000000, 0.000000000000000000 ) ) ;
#17270 = EDGE_CURVE ( 'NONE', #14460, #20150, #1053, .T. ) ;
#17271 = DIRECTION ( 'NONE',  ( -1.000000000000000000, 0.000000000000000000, -0.000000000000000000 ) ) ;
#17272 = VECTOR ( 'NONE', #3442, 1000.000000000000000 ) ;
#17273 = FACE_OUTER_BOUND ( 'NONE', #4325, .T. ) ;
#17274 = DIRECTION ( 'NONE',  ( 0.7705132427757999114, 0.6374239897486768669, 0.000000000000000000 ) ) ;
#17275 = VERTEX_POINT ( 'NONE', #21312 ) ;
#17276 = CARTESIAN_POINT ( 'NONE',  ( 3.756430356250003211, 29.30312499938548498, 8.999999999999992895 ) ) ;
#17277 = DIRECTION ( 'NONE',  ( 0.000000000000000000, 0.000000000000000000, 1.000000000000000000 ) ) ;
#17279 = VERTEX_POINT ( 'NONE', #18838 ) ;
#17278 = CARTESIAN_POINT ( 'NONE',  ( 0.000000000000000000, 0.000000000000000000, 1.000000000000000000 ) ) ;
#17280 = EDGE_CURVE ( 'NONE', #2220, #16594, #7904, .T. ) ;
#17281 = ORIENTED_EDGE ( 'NONE', *, *, #1835, .F. ) ;
#17282 = ORIENTED_EDGE ( 'NONE', *, *, #7691, .T. ) ;
#17283 = VERTEX_POINT ( 'NONE', #25108 ) ;
#17284 = ORIENTED_EDGE ( 'NONE', *, *, #14801, .T. ) ;
#17285 = CARTESIAN_POINT ( 'NONE',  ( 4.000000000000003553, -8.999999999999992895, 3.599999999999999201 ) ) ;
#17286 = LINE ( 'NONE', #13346, #16546 ) ;
#17287 = CARTESIAN_POINT ( 'NONE',  ( 3.756430356250006319, 25.17812499938548854, 6.831223922626973533 ) ) ;
#17288 = CARTESIAN_POINT ( 'NONE',  ( -3.756430356249996994, -8.999999999999992895, 4.078124999385482674 ) ) ;
#17289 = CARTESIAN_POINT ( 'NONE',  ( 2.620986760973688460E-15, -13.61880215351699874, 0.7312499987709674132 ) ) ;
#17290 = CARTESIAN_POINT ( 'NONE',  ( -3.756430356249995661, 25.89062499938548356, 6.831223922626973533 ) ) ;
#17291 = CYLINDRICAL_SURFACE ( 'NONE', #13819, 0.5000000000000004441 ) ;
#17292 = CARTESIAN_POINT ( 'NONE',  ( 21.05852382634284936, 21.05852382634277831, 12.99999999999999289 ) ) ;
#17293 = CARTESIAN_POINT ( 'NONE',  ( -3.756430356249996994, -8.999999999999992895, 3.965624999385481519 ) ) ;
#17294 = CYLINDRICAL_SURFACE ( 'NONE', #12960, 4.000000000000000000 ) ;
#17295 = FACE_OUTER_BOUND ( 'NONE', #1078, .T. ) ;
#17296 = FACE_OUTER_BOUND ( 'NONE', #14888, .T. ) ;
#17297 = CARTESIAN_POINT ( 'NONE',  ( -4.000000000000003553, -26.78124999877097068, 6.690598923241489970 ) ) ;
#17298 = CARTESIAN_POINT ( 'NONE',  ( 3.756430356250003655, -8.999999999999992895, 4.303124999385482319 ) ) ;
#17299 = CARTESIAN_POINT ( 'NONE',  ( 4.000000000000003553, -8.999999999999992895, 8.000000000000000000 ) ) ;
#17300 = EDGE_CURVE ( 'NONE', #11375, #18764, #15439, .T. ) ;
#17301 = CARTESIAN_POINT ( 'NONE',  ( -3.369928719974892281E-15, -25.11250000000000426, 4.999999999999992006 ) ) ;
#17302 = CYLINDRICAL_SURFACE ( 'NONE', #11812, 31.10000000000000142 ) ;
#17303 = ORIENTED_EDGE ( 'NONE', *, *, #21226, .F. ) ;
#17304 = CARTESIAN_POINT ( 'NONE',  ( -0.5000000000000000000, -2.999999999999999556, 20.00000000000000000 ) ) ;
#17305 = ORIENTED_EDGE ( 'NONE', *, *, #21354, .F. ) ;
#17306 = ADVANCED_FACE ( 'NONE', ( #20932 ), #3015, .T. ) ;
#17307 = ORIENTED_EDGE ( 'NONE', *, *, #3735, .F. ) ;
#17308 = DIRECTION ( 'NONE',  ( -0.9980267284282710039, 0.06279051952932233893, 0.000000000000000000 ) ) ;
#17309 = COLOUR_RGB ( '',0.8941176470588234615, 0.8941176470588234615, 0.8941176470588234615 ) ;
#17310 = ORIENTED_EDGE ( 'NONE', *, *, #21823, .T. ) ;
#17311 = CARTESIAN_POINT ( 'NONE',  ( 1.878215178124995832, -29.00312499938548427, 5.746835883940462963 ) ) ;
#17312 = ADVANCED_FACE ( 'NONE', ( #14792 ), #7058, .T. ) ;
#17313 = VERTEX_POINT ( 'NONE', #1308 ) ;
#17314 = DIRECTION ( 'NONE',  ( 0.000000000000000000, 0.000000000000000000, 1.000000000000000000 ) ) ;
#17315 = ORIENTED_EDGE ( 'NONE', *, *, #18142, .T. ) ;
#17316 = EDGE_CURVE ( 'NONE', #8421, #2048, #22766, .T. ) ;
#17317 = CARTESIAN_POINT ( 'NONE',  ( 2.620986760973688460E-15, 28.03750000000000142, 13.61880215351699874 ) ) ;
#17318 = FACE_OUTER_BOUND ( 'NONE', #16375, .T. ) ;
#17319 = PLANE ( 'NONE',  #10491 ) ;
#17320 = CARTESIAN_POINT ( 'NONE',  ( -3.999999999999996447, 25.63750000000000284, 6.690598923241487306 ) ) ;
#17321 = CARTESIAN_POINT ( 'NONE',  ( 19.28627369086489551, 21.94247106882419729, 12.25316411605951927 ) ) ;
#17322 = DIRECTION ( 'NONE',  ( 0.000000000000000000, 0.000000000000000000, 1.000000000000000000 ) ) ;
#17323 = EDGE_CURVE ( 'NONE', #19968, #12673, #20017, .T. ) ;
#17324 = CARTESIAN_POINT ( 'NONE',  ( -3.999999999999997335, 25.71250000000000213, 11.30940107675849404 ) ) ;
#17325 = CARTESIAN_POINT ( 'NONE',  ( 19.36809667800328683, 19.36809667800321577, 13.33755215474603162 ) ) ;
#17326 = CARTESIAN_POINT ( 'NONE',  ( 6.317933499823220167, -30.45149776762731975, 1.000000000000000000 ) ) ;
#17327 = ORIENTED_EDGE ( 'NONE', *, *, #23484, .F. ) ;
#17328 = VERTEX_POINT ( 'NONE', #7198 ) ;
#17329 = CARTESIAN_POINT ( 'NONE',  ( -1.999999999999994893, 28.24374999877096926, 5.535898384862237620 ) ) ;
#17330 = CARTESIAN_POINT ( 'NONE',  ( -14.48253926456356666, -27.25313774936403988, -6.500000000000000000 ) ) ;
#17331 = ORIENTED_EDGE ( 'NONE', *, *, #24471, .F. ) ;
#17332 = CARTESIAN_POINT ( 'NONE',  ( 0.000000000000000000, 20.00000000000000000, 17.69999999999999929 ) ) ;
#17333 = CARTESIAN_POINT ( 'NONE',  ( -3.756430356249997882, 28.66562499938548569, 11.16877607737301226 ) ) ;
#17334 = DIRECTION ( 'NONE',  ( 0.000000000000000000, 1.000000000000000000, 0.000000000000000000 ) ) ;
#17335 = ORIENTED_EDGE ( 'NONE', *, *, #932, .F. ) ;
#17336 = EDGE_CURVE ( 'NONE', #24543, #13216, #7494, .T. ) ;
#17337 = ORIENTED_EDGE ( 'NONE', *, *, #9365, .T. ) ;
#17338 = CARTESIAN_POINT ( 'NONE',  ( -23.96296185032681336, 19.82388608118453632, -6.500000000000000000 ) ) ;
#17339 = CARTESIAN_POINT ( 'NONE',  ( 0.000000000000000000, 0.000000000000000000, -6.500000000000000000 ) ) ;
#17340 = EDGE_LOOP ( 'NONE', ( #7355, #3013, #14732, #786 ) ) ;
#17341 = EDGE_CURVE ( 'NONE', #17107, #6707, #16690, .T. ) ;
#17342 = CARTESIAN_POINT ( 'NONE',  ( -1.878215178125000939, -28.32812499938548711, 12.25316411605952283 ) ) ;
#17343 = CARTESIAN_POINT ( 'NONE',  ( 5.577813053751546416E-15, 25.33750000000000213, 12.99999999999999289 ) ) ;
#17344 = CARTESIAN_POINT ( 'NONE',  ( -3.756430356249994773, 28.06562499938548783, 8.999999999999992895 ) ) ;
#17345 = EDGE_CURVE ( 'NONE', #13848, #14914, #15029, .T. ) ;
#17346 = CARTESIAN_POINT ( 'NONE',  ( 29.41953157733093960, 10.08469938919488484, -2.750000000000000000 ) ) ;
#17347 = CARTESIAN_POINT ( 'NONE',  ( 4.000000000000005329, 25.03750000000000142, 6.690598923241489970 ) ) ;
#17348 = APPLICATION_PROTOCOL_DEFINITION ( 'draft international standard', 'automotive_design', 1998, #3250 ) ;
#17349 = CARTESIAN_POINT ( 'NONE',  ( -0.4999838450259763700, -31.09598070739550124, -2.750000000000000000 ) ) ;
#17350 = CYLINDRICAL_SURFACE ( 'NONE', #6310, 0.5000000000000004441 ) ;
#17351 = CARTESIAN_POINT ( 'NONE',  ( 1.878215178125004048, 27.46562499938548640, 5.746835883940462963 ) ) ;
#17352 = CARTESIAN_POINT ( 'NONE',  ( -1.057460391440397258E-14, 29.16249999999999787, 4.999999999999992006 ) ) ;
#17353 = CARTESIAN_POINT ( 'NONE',  ( 22.02202058170775345, 19.36582320374829891, 5.746835883940462963 ) ) ;
#17354 = CARTESIAN_POINT ( 'NONE',  ( 17.90741546755112523, 20.56361284551042701, 5.746835883940462963 ) ) ;
#17355 = CARTESIAN_POINT ( 'NONE',  ( 17.60253943329360382, 20.43096655803972084, 5.535898384862237620 ) ) ;
#17356 = CARTESIAN_POINT ( 'NONE',  ( 0.7500000000000000000, -2.999999999999999556, 18.19999999999999929 ) ) ;
#17357 = CARTESIAN_POINT ( 'NONE',  ( -3.999999999999996447, -8.999999999999992895, 18.00000000000000000 ) ) ;
#17358 = CARTESIAN_POINT ( 'NONE',  ( 18.81125008781888042, 18.81125008781880581, 4.662447845253954171 ) ) ;
#17359 = CYLINDRICAL_SURFACE ( 'NONE', #12119, 4.000000000000000000 ) ;
#17360 = ORIENTED_EDGE ( 'NONE', *, *, #12071, .T. ) ;
#17361 = CARTESIAN_POINT ( 'NONE',  ( 4.000000000000001776, 25.80624999877096926, 11.30940107675849760 ) ) ;
#17362 = CARTESIAN_POINT ( 'NONE',  ( -1.878215178124995832, 25.85312499938548569, 5.746835883940462963 ) ) ;
#17363 = CARTESIAN_POINT ( 'NONE',  ( -3.752267015613588906E-15, -25.11250000000000071, 4.381197846482986158 ) ) ;
#17365 = ORIENTED_EDGE ( 'NONE', *, *, #7727, .T. ) ;
#17364 = CARTESIAN_POINT ( 'NONE',  ( 8.012344526598182026E-15, 25.81562499938549138, 4.662447845253954171 ) ) ;
#17366 = CARTESIAN_POINT ( 'NONE',  ( 2.672651547586948120E-15, 26.04062499938548925, 13.33755215474603162 ) ) ;
#17367 = CARTESIAN_POINT ( 'NONE',  ( 6.972266317189432034E-15, 28.65624999877097423, 4.999999999999992006 ) ) ;
#17368 = CARTESIAN_POINT ( 'NONE',  ( -1.878215178125004048, -28.36562499938548143, 5.746835883940462963 ) ) ;
#17369 = VERTEX_POINT ( 'NONE', #5615 ) ;
#17370 = ORIENTED_EDGE ( 'NONE', *, *, #4364, .T. ) ;
#17371 = DIRECTION ( 'NONE',  ( 0.000000000000000000, 0.000000000000000000, 1.000000000000000000 ) ) ;
#17372 = CARTESIAN_POINT ( 'NONE',  ( 3.756430356250004543, 29.34062499938548640, 6.831223922626973533 ) ) ;
#17373 = ADVANCED_FACE ( 'NONE', ( #15808 ), #13596, .T. ) ;
#17374 = CARTESIAN_POINT ( 'NONE',  ( -8.217531866531428975, -29.99470236596023653, -2.750000000000000000 ) ) ;
#17375 = EDGE_CURVE ( 'NONE', #9259, #15106, #19606, .T. ) ;
#17376 = CARTESIAN_POINT ( 'NONE',  ( -3.756430356249995661, -6.831223922626973533, 4.040624999385483918 ) ) ;
#17377 = CARTESIAN_POINT ( 'NONE',  ( 3.469446951953614189E-15, -8.999999999999992895, 18.00000000000000000 ) ) ;
#17378 = DIRECTION ( 'NONE',  ( 1.000000000000000000, 0.000000000000000000, 0.000000000000000000 ) ) ;
#17379 = CARTESIAN_POINT ( 'NONE',  ( -27.10000000000000497, -0.5999999999999998668, 19.00000000000000000 ) ) ;
#17380 = DIRECTION ( 'NONE',  ( -0.000000000000000000, -0.000000000000000000, -1.000000000000000000 ) ) ;
#17381 = LINE ( 'NONE', #16998, #12049 ) ;
#17382 = DIRECTION ( 'NONE',  ( 0.000000000000000000, -0.000000000000000000, 1.000000000000000000 ) ) ;
#17383 = ORIENTED_EDGE ( 'NONE', *, *, #14254, .F. ) ;
#17384 = DIRECTION ( 'NONE',  ( 0.000000000000000000, 0.000000000000000000, 1.000000000000000000 ) ) ;
#17385 = CARTESIAN_POINT ( 'NONE',  ( -5.827558883616271501, -30.54913349766217934, -6.500000000000000000 ) ) ;
#17386 = DIRECTION ( 'NONE',  ( 0.000000000000000000, 0.000000000000000000, 1.000000000000000000 ) ) ;
#17387 = DIRECTION ( 'NONE',  ( -0.000000000000000000, 1.000000000000000000, 0.000000000000000000 ) ) ;
#17388 = CARTESIAN_POINT ( 'NONE',  ( -3.526711513754876570, 29.50000000000000000, 4.145898033750337497 ) ) ;
#17389 = CARTESIAN_POINT ( 'NONE',  ( -1.071796769724492338, -28.50759618943233775, 12.99999999999999467 ) ) ;
#17390 = ORIENTED_EDGE ( 'NONE', *, *, #9072, .T. ) ;
#17391 = CARTESIAN_POINT ( 'NONE',  ( 1.071796769724494558, 27.34240381056766722, 4.999999999999992895 ) ) ;
#17392 = CARTESIAN_POINT ( 'NONE',  ( -3.401318489841309578, -30.91344420362545264, 1.000000000000000000 ) ) ;
#17394 = ORIENTED_EDGE ( 'NONE', *, *, #20992, .F. ) ;
#17393 = CARTESIAN_POINT ( 'NONE',  ( 3.999999999999996447, -26.51874999877097139, 8.999999999999992895 ) ) ;
#17395 = ORIENTED_EDGE ( 'NONE', *, *, #18302, .F. ) ;
#17396 = ORIENTED_EDGE ( 'NONE', *, *, #10383, .T. ) ;
#17397 = ORIENTED_EDGE ( 'NONE', *, *, #2406, .F. ) ;
#17398 = VERTEX_POINT ( 'NONE', #21563 ) ;
#17399 = EDGE_CURVE ( 'NONE', #10033, #7472, #22530, .T. ) ;
#17400 = CARTESIAN_POINT ( 'NONE',  ( 31.00322564728514152, -2.451530025009115654, 1.000000000000000000 ) ) ;
#17401 = DIRECTION ( 'NONE',  ( 0.000000000000000000, 0.000000000000000000, -1.000000000000000000 ) ) ;
#17402 = EDGE_CURVE ( 'NONE', #15841, #32, #21985, .T. ) ;
#17403 = CARTESIAN_POINT ( 'NONE',  ( 1.878215178124998275, 25.51562499938548711, 12.25316411605952283 ) ) ;
#17404 = CARTESIAN_POINT ( 'NONE',  ( -3.756430356249995661, -6.831223922626973533, 1.678124999385481875 ) ) ;
#17405 = CARTESIAN_POINT ( 'NONE',  ( -3.999999999999996447, -8.999999999999992895, 2.418749998770966414 ) ) ;
#17406 = PRODUCT_DEFINITION_SHAPE ( 'NONE', 'NONE',  #25884 ) ;
#17407 =( NAMED_UNIT ( * ) PLANE_ANGLE_UNIT ( ) SI_UNIT ( $, .RADIAN. ) );
#17408 = CARTESIAN_POINT ( 'NONE',  ( -1.878215178124995832, 27.20312499938548711, 5.746835883940462963 ) ) ;
#17409 = EDGE_CURVE ( 'NONE', #7828, #13988, #9605, .T. ) ;
#17410 = CARTESIAN_POINT ( 'NONE',  ( -3.999999999999997335, -11.30940107675849404, 3.806249998770963927 ) ) ;
#17411 = LINE ( 'NONE', #7458, #16385 ) ;
#17412 = CARTESIAN_POINT ( 'NONE',  ( -3.999999999999997335, -11.30940107675849404, 2.512500000000001510 ) ) ;
#17413 = DIRECTION ( 'NONE',  ( 0.000000000000000000, -1.000000000000000000, 0.000000000000000000 ) ) ;
#17414 = DIRECTION ( 'NONE',  ( 1.000000000000000000, 0.000000000000000000, 0.000000000000000000 ) ) ;
#17415 = DIRECTION ( 'NONE',  ( 0.000000000000000000, 0.000000000000000000, 1.000000000000000000 ) ) ;
#17416 = CARTESIAN_POINT ( 'NONE',  ( -4.000000000000003553, -25.84374999877096712, 8.999999999999992895 ) ) ;
#17417 = CARTESIAN_POINT ( 'NONE',  ( 3.756430356250002323, -11.16877607737301403, 4.265624999385481786 ) ) ;
#17418 = LINE ( 'NONE', #19490, #23309 ) ;
#17419 = LINE ( 'NONE', #22695, #12465 ) ;
#17420 = CARTESIAN_POINT ( 'NONE',  ( -1.071796769724494558, -25.99240381056766580, 4.999999999999992895 ) ) ;
#17421 = ORIENTED_EDGE ( 'NONE', *, *, #18449, .F. ) ;
#17422 = DIRECTION ( 'NONE',  ( 1.000000000000000000, 0.000000000000000000, 0.000000000000000000 ) ) ;
#17423 = VERTEX_POINT ( 'NONE', #1561 ) ;
#17424 = ORIENTED_EDGE ( 'NONE', *, *, #12141, .F. ) ;
#17425 = DIRECTION ( 'NONE',  ( -0.000000000000000000, 1.000000000000000000, -0.000000000000000000 ) ) ;
#17426 = ORIENTED_EDGE ( 'NONE', *, *, #23054, .F. ) ;
#17427 = CARTESIAN_POINT ( 'NONE',  ( -2.672651547586948120E-15, -29.19062499938548783, 13.33755215474602984 ) ) ;
#17428 = EDGE_LOOP ( 'NONE', ( #21863, #16622, #5856, #4096 ) ) ;
#17429 = CARTESIAN_POINT ( 'NONE',  ( -1.057460391440397258E-14, 28.71250000000000213, 4.999999999999992006 ) ) ;
#17430 = ORIENTED_EDGE ( 'NONE', *, *, #11951, .F. ) ;
#17431 = CARTESIAN_POINT ( 'NONE',  ( 2.000000000000003997, 27.32500000000000284, 5.535898384862238508 ) ) ;
#17432 = CARTESIAN_POINT ( 'NONE',  ( 20.10392967174102097, 20.10392967174092860, 12.99999999999999289 ) ) ;
#17433 = EDGE_CURVE ( 'NONE', #10990, #19250, #18349, .T. ) ;
#17434 = DIRECTION ( 'NONE',  ( -0.9685831611286319642, -0.2486898871648515197, 0.000000000000000000 ) ) ;
#17435 = DIRECTION ( 'NONE',  ( 0.000000000000000000, 0.000000000000000000, 1.000000000000000000 ) ) ;
#17436 = CARTESIAN_POINT ( 'NONE',  ( 20.64088888413906986, 20.64088888413900236, 13.33755215474602984 ) ) ;
#17437 = DIRECTION ( 'NONE',  ( 0.000000000000000000, -0.000000000000000000, -1.000000000000000000 ) ) ;
#17438 = CARTESIAN_POINT ( 'NONE',  ( -1.999999999999995781, 26.95000000000000284, 5.535898384862237620 ) ) ;
#17439 = CARTESIAN_POINT ( 'NONE',  ( 15.70427213685309020, 21.01666689277176658, 11.16877607737301048 ) ) ;
#17440 = CARTESIAN_POINT ( 'NONE',  ( -30.53863125411927371, -1.952785157361310198, 1.000000000000000000 ) ) ;
#17441 = ORIENTED_EDGE ( 'NONE', *, *, #6970, .F. ) ;
#17442 = VERTEX_POINT ( 'NONE', #9530 ) ;
#17443 = CARTESIAN_POINT ( 'NONE',  ( 4.000000000000000888, 28.95624999877097494, 11.30940107675849760 ) ) ;
#17444 = LINE ( 'NONE', #8129, #25012 ) ;
#17445 = ORIENTED_EDGE ( 'NONE', *, *, #25119, .T. ) ;
#17446 = FACE_OUTER_BOUND ( 'NONE', #17844, .T. ) ;
#17447 = CARTESIAN_POINT ( 'NONE',  ( 3.756430356250003655, 28.85312499938548569, 8.999999999999992895 ) ) ;
#17448 = PLANE ( 'NONE',  #2961 ) ;
#17449 = ORIENTED_EDGE ( 'NONE', *, *, #16510, .T. ) ;
#17450 = ORIENTED_EDGE ( 'NONE', *, *, #11626, .F. ) ;
#17451 = VECTOR ( 'NONE', #25608, 1000.000000000000000 ) ;
#17452 = CARTESIAN_POINT ( 'NONE',  ( -1.859271017917182139E-15, -29.78124999877096712, 12.99999999999999289 ) ) ;
#17453 = ORIENTED_EDGE ( 'NONE', *, *, #20383, .T. ) ;
#17454 = CARTESIAN_POINT ( 'NONE',  ( 3.289814793420742678, 38.99786504297400569, 4.589397325852536014 ) ) ;
#17455 = CARTESIAN_POINT ( 'NONE',  ( -1.878215178124995832, 25.74062499938548498, 5.746835883940462963 ) ) ;
#17456 = CARTESIAN_POINT ( 'NONE',  ( -3.756430356249996549, 27.12812499938548783, 6.831223922626973533 ) ) ;
#17457 = DIRECTION ( 'NONE',  ( 0.000000000000000000, 0.000000000000000000, 1.000000000000000000 ) ) ;
#17458 = CARTESIAN_POINT ( 'NONE',  ( 4.000000000000001776, 26.35000000000000497, 8.999999999999992895 ) ) ;
#17459 = EDGE_CURVE ( 'NONE', #3291, #24428, #12284, .T. ) ;
#17460 = CARTESIAN_POINT ( 'NONE',  ( 1.878215178125000939, 28.21562499938548640, 12.25316411605952283 ) ) ;
#17461 = ADVANCED_FACE ( 'NONE', ( #7576 ), #19734, .F. ) ;
#17462 = CARTESIAN_POINT ( 'NONE',  ( 21.21320343559646915, 21.21320343559638744, 4.999999999999992006 ) ) ;
#17463 = LINE ( 'NONE', #19039, #10484 ) ;
#17464 = VECTOR ( 'NONE', #25138, 1000.000000000000000 ) ;
#17465 = CARTESIAN_POINT ( 'NONE',  ( -3.756430356249997438, 26.75312499938548427, 11.16877607737301048 ) ) ;
#17466 = CARTESIAN_POINT ( 'NONE',  ( -3.469446951953614189E-15, -30.00000000000000355, 4.999999999999992006 ) ) ;
#17467 = CARTESIAN_POINT ( 'NONE',  ( 19.66640735175089461, 19.66640735175081645, 4.381197846482986158 ) ) ;
#17468 = CARTESIAN_POINT ( 'NONE',  ( 17.58694394176227149, 22.89933869768094610, 8.999999999999992895 ) ) ;
#17469 = EDGE_CURVE ( 'NONE', #19944, #9003, #17944, .T. ) ;
#17470 = DIRECTION ( 'NONE',  ( 0.000000000000000000, 0.000000000000000000, 1.000000000000000000 ) ) ;
#17471 =( BOUNDED_CURVE ( )  B_SPLINE_CURVE ( 2, ( #11676, #3966, #7634, #13646, #10103, #13527, #1613, #23703, #8152 ),
 .UNSPECIFIED., .F., .F. ) 
 B_SPLINE_CURVE_WITH_KNOTS ( ( 3, 2, 2, 2, 3 ),
 ( 0.6750000000000000444, 0.6833333333333333481, 0.6999999999999999556, 0.7166666666666666741, 0.7249999999999999778 ),
 .UNSPECIFIED. ) 
 CURVE ( )  GEOMETRIC_REPRESENTATION_ITEM ( )  RATIONAL_B_SPLINE_CURVE ( ( 0.9330127018922194093, 0.9330127018922198534, 1.000000000000000000, 0.8660254037844387076, 1.000000000000000000, 0.8660254037844387076, 1.000000000000000000, 0.9330127018922194093, 0.9330127018922194093 ) ) 
 REPRESENTATION_ITEM ( '' )  );
#17472 = DIRECTION ( 'NONE',  ( 0.000000000000000000, 0.000000000000000000, 1.000000000000000000 ) ) ;
#17473 = LINE ( 'NONE', #17357, #19157 ) ;
#17474 = CARTESIAN_POINT ( 'NONE',  ( 19.44764619088677904, 19.44764619088670088, 4.662447845253954171 ) ) ;
#17475 = DIRECTION ( 'NONE',  ( -0.000000000000000000, -1.000000000000000000, -0.000000000000000000 ) ) ;
#17476 = ORIENTED_EDGE ( 'NONE', *, *, #1169, .F. ) ;
#17477 = DIRECTION ( 'NONE',  ( 1.000000000000000000, 0.000000000000000000, 0.000000000000000000 ) ) ;
#17478 = CARTESIAN_POINT ( 'NONE',  ( -2.000000000000003997, -25.97500000000000142, 5.535898384862238508 ) ) ;
#17480 = ORIENTED_EDGE ( 'NONE', *, *, #14772, .F. ) ;
#17479 = CARTESIAN_POINT ( 'NONE',  ( -27.49048467073837898, 14.54246377227389075, -2.750000000000000000 ) ) ;
#17481 = CARTESIAN_POINT ( 'NONE',  ( -1.878215178124995832, 25.85312499938548569, 5.746835883940462963 ) ) ;
#17482 = CARTESIAN_POINT ( 'NONE',  ( 9.133673601486375304, -29.72853858738285027, 1.000000000000000000 ) ) ;
#17483 = ORIENTED_EDGE ( 'NONE', *, *, #16969, .F. ) ;
#17484 = CARTESIAN_POINT ( 'NONE',  ( 3.756430356249995661, -28.02812499938548640, 6.831223922626973533 ) ) ;
#17485 = ORIENTED_EDGE ( 'NONE', *, *, #3058, .T. ) ;
#17486 = EDGE_LOOP ( 'NONE', ( #19816, #19555 ) ) ;
#17487 = CARTESIAN_POINT ( 'NONE',  ( -3.756430356249998326, 25.85312499938549635, 11.16877607737301226 ) ) ;
#17488 = AXIS2_PLACEMENT_3D ( 'NONE', #14062, #2167, #19683 ) ;
#17489 = CARTESIAN_POINT ( 'NONE',  ( -1.878215178124998497, -12.25316411605951927, 0.4406249993854846614 ) ) ;
#17490 = VECTOR ( 'NONE', #13021, 1000.000000000000000 ) ;
#17491 = CIRCLE ( 'NONE', #6209, 31.10000000000000142 ) ;
#17492 = CARTESIAN_POINT ( 'NONE',  ( -1.878215178124998497, -12.25316411605951927, 3.703124999385482674 ) ) ;
#17493 = CARTESIAN_POINT ( 'NONE',  ( 3.137519842735244810E-15, -27.30624999877096926, 4.999999999999991118 ) ) ;
#17494 = DIRECTION ( 'NONE',  ( 0.000000000000000000, 0.000000000000000000, 1.000000000000000000 ) ) ;
#17495 = CYLINDRICAL_SURFACE ( 'NONE', #3804, 0.5000000000000004441 ) ;
#17496 = DIRECTION ( 'NONE',  ( 1.000000000000000000, 0.000000000000000000, -0.000000000000000000 ) ) ;
#17497 = CARTESIAN_POINT ( 'NONE',  ( 2.000000000000003997, 25.91874999877096997, 5.535898384862238508 ) ) ;
#17498 = CARTESIAN_POINT ( 'NONE',  ( 2.451530025009136970, 31.00322564728514152, -2.750000000000000000 ) ) ;
#17499 = DIRECTION ( 'NONE',  ( 0.000000000000000000, 1.000000000000000000, 0.000000000000000000 ) ) ;
#17500 = EDGE_CURVE ( 'NONE', #7090, #22371, #14189, .T. ) ;
#17501 = ORIENTED_EDGE ( 'NONE', *, *, #10900, .F. ) ;
#17502 = CARTESIAN_POINT ( 'NONE',  ( 3.469446951953614189E-15, 40.00000000000000000, 8.999999999999992895 ) ) ;
#17503 = CARTESIAN_POINT ( 'NONE',  ( -1.878215178125000939, -29.67812499938548498, 12.25316411605952283 ) ) ;
#17504 = CARTESIAN_POINT ( 'NONE',  ( 3.756430356250003655, 26.60312499938548569, 8.999999999999992895 ) ) ;
#17505 = ADVANCED_FACE ( 'NONE', ( #4160 ), #4687, .F. ) ;
#17506 = FACE_OUTER_BOUND ( 'NONE', #25628, .T. ) ;
#17507 = AXIS2_PLACEMENT_3D ( 'NONE', #3605, #13808, #25322 ) ;
#17508 = CARTESIAN_POINT ( 'NONE',  ( 4.648177544792955347E-16, 28.93750000000000355, 12.99999999999999289 ) ) ;
#17509 = CARTESIAN_POINT ( 'NONE',  ( 4.000000000000003553, 28.99374999877096926, 8.999999999999992895 ) ) ;
#17510 = EDGE_LOOP ( 'NONE', ( #10326, #2080, #18464, #16716 ) ) ;
#17511 = CARTESIAN_POINT ( 'NONE',  ( -3.756430356250000546, 29.56562499938549493, 11.16877607737301226 ) ) ;
#17512 = CARTESIAN_POINT ( 'NONE',  ( -5.218519194534875894, 39.00427158776031433, 7.275297520595652045 ) ) ;
#17514 = EDGE_LOOP ( 'NONE', ( #22014, #23955, #13749, #7263 ) ) ;
#17513 = CARTESIAN_POINT ( 'NONE',  ( -1.071796769724491227, -26.44240381056766509, 4.999999999999989342 ) ) ;
#17515 = EDGE_CURVE ( 'NONE', #15910, #23645, #12136, .T. ) ;
#17516 = CIRCLE ( 'NONE', #6225, 0.7500000000000001110 ) ;
#17517 = EDGE_LOOP ( 'NONE', ( #5707, #12675, #14497, #13753 ) ) ;
#17519 = EDGE_LOOP ( 'NONE', ( #11426, #8998, #18468, #6818 ) ) ;
#17518 = VECTOR ( 'NONE', #3939, 1000.000000000000000 ) ;
#17520 = ORIENTED_EDGE ( 'NONE', *, *, #5020, .T. ) ;
#17521 = ORIENTED_EDGE ( 'NONE', *, *, #44, .F. ) ;
#17522 = CYLINDRICAL_SURFACE ( 'NONE', #12634, 31.10000000000000142 ) ;
#17523 = DIRECTION ( 'NONE',  ( 0.000000000000000000, 0.000000000000000000, 1.000000000000000000 ) ) ;
#17524 = EDGE_CURVE ( 'NONE', #6543, #9952, #12496, .T. ) ;
#17525 = CIRCLE ( 'NONE', #17957, 31.10000000000000142 ) ;
#17526 = CYLINDRICAL_SURFACE ( 'NONE', #10562, 31.10000000000000142 ) ;
#17527 = AXIS2_PLACEMENT_3D ( 'NONE', #1813, #12253, #17755 ) ;
#17528 = AXIS2_PLACEMENT_3D ( 'NONE', #14624, #22604, #129 ) ;
#17529 = CARTESIAN_POINT ( 'NONE',  ( 1.878215178125000939, -12.25316411605952283, 1.865624999385483873 ) ) ;
#17530 = CARTESIAN_POINT ( 'NONE',  ( 3.752267015613588906E-15, -4.381197846482986158, 2.306249998770968368 ) ) ;
#17531 = SHAPE_REPRESENTATION_RELATIONSHIP ( 'NONE' , 'NONE' ,  #16033, #14134 ) ;
#17532 = CARTESIAN_POINT ( 'NONE',  ( 1.878215178125000939, 27.87812499938548427, 12.25316411605952283 ) ) ;
#17533=STYLED_ITEM('',(#25900),#22081);
#17534 = CARTESIAN_POINT ( 'NONE',  ( -1.071796769724495668, -26.65134618820330203, 12.99999999999999112 ) ) ;
#17535 = DIRECTION ( 'NONE',  ( 0.000000000000000000, -1.000000000000000000, -0.000000000000000000 ) ) ;
#17536 = AXIS2_PLACEMENT_3D ( 'NONE', #332, #14339, #2413 ) ;
#17537 = EDGE_CURVE ( 'NONE', #27, #7266, #12935, .T. ) ;
#17538 = CARTESIAN_POINT ( 'NONE',  ( -3.999999999999996447, -8.999999999999992895, 2.024999999999999023 ) ) ;
#17539 = DIRECTION ( 'NONE',  ( -0.000000000000000000, -0.000000000000000000, -1.000000000000000000 ) ) ;
#17540 = LINE ( 'NONE', #1191, #5360 ) ;
#17541 = CARTESIAN_POINT ( 'NONE',  ( 21.28941499438209206, -22.67092431280601872, -6.500000000000000000 ) ) ;
#17542 = CARTESIAN_POINT ( 'NONE',  ( -2.000000000000003997, -26.36874999877096926, 5.535898384862238508 ) ) ;
#17543 = CARTESIAN_POINT ( 'NONE',  ( -3.756430356249995661, 28.14062499938548356, 6.831223922626973533 ) ) ;
#17544 = ADVANCED_FACE ( 'NONE', ( #8485 ), #20113, .T. ) ;
#17545 = DIRECTION ( 'NONE',  ( -0.1873813145857259888, -0.9822872507286884991, 0.000000000000000000 ) ) ;
#17546 = AXIS2_PLACEMENT_3D ( 'NONE', #10043, #1949, #8099 ) ;
#17547 = DIRECTION ( 'NONE',  ( 0.000000000000000000, 0.000000000000000000, 1.000000000000000000 ) ) ;
#17548 = CARTESIAN_POINT ( 'NONE',  ( 16.66421332384682685, 26.25859848311265310, -6.500000000000000000 ) ) ;
#17549 = ORIENTED_EDGE ( 'NONE', *, *, #15566, .T. ) ;
#17550 = DIRECTION ( 'NONE',  ( 0.000000000000000000, 0.000000000000000000, 1.000000000000000000 ) ) ;
#17551 = ORIENTED_EDGE ( 'NONE', *, *, #25505, .T. ) ;
#17552 = ORIENTED_EDGE ( 'NONE', *, *, #18420, .T. ) ;
#17553 = CARTESIAN_POINT ( 'NONE',  ( 0.000000000000000000, 0.000000000000000000, -6.500000000000000000 ) ) ;
#17554 = ORIENTED_EDGE ( 'NONE', *, *, #3022, .F. ) ;
#17555 = CARTESIAN_POINT ( 'NONE',  ( -3.756430356250002323, -27.01562499938548356, 11.16877607737301226 ) ) ;
#17556 = ORIENTED_EDGE ( 'NONE', *, *, #1842, .F. ) ;
#17557 = VERTEX_POINT ( 'NONE', #14107 ) ;
#17558 = CARTESIAN_POINT ( 'NONE',  ( 1.071796769724491227, 26.89240381056766793, 4.999999999999989342 ) ) ;
#17559 = ADVANCED_FACE ( 'NONE', ( #10559 ), #22071, .T. ) ;
#17560 = EDGE_LOOP ( 'NONE', ( #8946, #24612, #19493, #14662 ) ) ;
#17561 = CARTESIAN_POINT ( 'NONE',  ( -3.999999999999997335, 26.16250000000000142, 11.30940107675849404 ) ) ;
#17562 = FACE_OUTER_BOUND ( 'NONE', #22764, .T. ) ;
#17563 = AXIS2_PLACEMENT_3D ( 'NONE', #4387, #12368, #18258 ) ;
#17564 = CARTESIAN_POINT ( 'NONE',  ( 3.756430356250003655, -8.999999999999992895, 1.153124999385485960 ) ) ;
#17565 = CARTESIAN_POINT ( 'NONE',  ( -31.06601413805600842, 1.453535542772947942, -6.500000000000000000 ) ) ;
#17566 = CARTESIAN_POINT ( 'NONE',  ( 23.69483382651587888, 18.38243907059705151, 8.999999999999992895 ) ) ;
#17567 = AXIS2_PLACEMENT_3D ( 'NONE', #6529, #17919, #10 ) ;
#17568 = CYLINDRICAL_SURFACE ( 'NONE', #21338, 4.000000000000000000 ) ;
#17569 = AXIS2_PLACEMENT_3D ( 'NONE', #24684, #3105, #12911 ) ;
#17570 = CARTESIAN_POINT ( 'NONE',  ( 4.000000000000001776, 28.56249999999999645, 11.30940107675849760 ) ) ;
#17571 = CIRCLE ( 'NONE', #13416, 0.4999999999999997224 ) ;
#17572 = CARTESIAN_POINT ( 'NONE',  ( 1.859271017917182139E-15, 25.78750000000000142, 12.99999999999999289 ) ) ;
#17573 = DIRECTION ( 'NONE',  ( 0.000000000000000000, 0.000000000000000000, 1.000000000000000000 ) ) ;
#17574 = VERTEX_POINT ( 'NONE', #4301 ) ;
#17575 = ORIENTED_EDGE ( 'NONE', *, *, #15019, .T. ) ;
#17576 = CARTESIAN_POINT ( 'NONE',  ( -2.003086131649545506E-15, 29.78124999877097778, 13.61880215351699874 ) ) ;
#17577 = ADVANCED_FACE ( 'NONE', ( #24303 ), #24432, .T. ) ;
#17578 = ORIENTED_EDGE ( 'NONE', *, *, #8912, .T. ) ;
#17579 = CARTESIAN_POINT ( 'NONE',  ( 1.859271017917182139E-15, 29.78124999877096712, 12.99999999999999289 ) ) ;
#17580 = AXIS2_PLACEMENT_3D ( 'NONE', #14048, #22400, #22279 ) ;
#17581 = CARTESIAN_POINT ( 'NONE',  ( 3.756430356250002323, 28.36562499938548854, 11.16877607737301226 ) ) ;
#17582 = CARTESIAN_POINT ( 'NONE',  ( -3.999999999999996447, 27.41874999877096641, 8.999999999999992895 ) ) ;
#17583 = ORIENTED_EDGE ( 'NONE', *, *, #22622, .T. ) ;
#17584 = EDGE_LOOP ( 'NONE', ( #21833, #13296, #4878, #11230 ) ) ;
#17585 = VECTOR ( 'NONE', #4806, 1000.000000000000000 ) ;
#17586 = AXIS2_PLACEMENT_3D ( 'NONE', #2509, #8401, #6436 ) ;
#17587 = DIRECTION ( 'NONE',  ( 1.000000000000000000, 0.000000000000000000, 0.000000000000000000 ) ) ;
#17588 = VERTEX_POINT ( 'NONE', #16195 ) ;
#17589 = DIRECTION ( 'NONE',  ( 1.000000000000000000, 0.000000000000000000, 0.000000000000000000 ) ) ;
#17590 = CARTESIAN_POINT ( 'NONE',  ( 2.672651547586948120E-15, 25.92812499938548498, 13.33755215474602984 ) ) ;
#17591 = CARTESIAN_POINT ( 'NONE',  ( -1.878215178124996498, 28.89062499938548711, 5.746835883940462963 ) ) ;
#17592 = CARTESIAN_POINT ( 'NONE',  ( 0.4553717634079643695, 38.72245023127408814, 3.239938118008596213 ) ) ;
#17593 = CARTESIAN_POINT ( 'NONE',  ( 2.003086131649545506E-15, 27.58750000000000568, 13.61880215351699874 ) ) ;
#17594 = CARTESIAN_POINT ( 'NONE',  ( -3.756430356249997882, 29.45312499938548356, 11.16877607737301226 ) ) ;
#17595 = FACE_OUTER_BOUND ( 'NONE', #23329, .T. ) ;
#17596 = DIRECTION ( 'NONE',  ( -1.000000000000000000, 0.000000000000000000, 0.000000000000000000 ) ) ;
#17597 = CARTESIAN_POINT ( 'NONE',  ( -3.756430356249996994, 28.96562499938548285, 8.999999999999992895 ) ) ;
#17598 = CARTESIAN_POINT ( 'NONE',  ( -3.013468763610312351, -29.84883905190463338, 6.356741067357151387 ) ) ;
#17599 = CARTESIAN_POINT ( 'NONE',  ( 20.31164228958361306, 17.48321516483735394, 12.46410161513774817 ) ) ;
#17600 = CARTESIAN_POINT ( 'NONE',  ( 20.00449278107117834, 20.00449278107111084, 13.33755215474602984 ) ) ;
#17601 = CARTESIAN_POINT ( 'NONE',  ( 0.000000000000000000, 0.000000000000000000, -6.500000000000000000 ) ) ;
#17602 = DIRECTION ( 'NONE',  ( 0.000000000000000000, 0.000000000000000000, -1.000000000000000000 ) ) ;
#17603 = CIRCLE ( 'NONE', #10914, 5.000000000000000888 ) ;
#17604 = CARTESIAN_POINT ( 'NONE',  ( 28.14012133169324414, 13.24173596767369254, -6.500000000000000000 ) ) ;
#17605 = EDGE_CURVE ( 'NONE', #18353, #18087, #2585, .T. ) ;
#17606 = CARTESIAN_POINT ( 'NONE',  ( 21.59775651299582222, 18.94155913503637478, 12.25316411605952283 ) ) ;
#17607 = CARTESIAN_POINT ( 'NONE',  ( 3.469446951953614189E-15, 30.00000000000000355, 4.999999999999992006 ) ) ;
#17608 = VERTEX_POINT ( 'NONE', #4420 ) ;
#17609 = CARTESIAN_POINT ( 'NONE',  ( -3.137519842735244810E-15, 26.85624999877096641, 4.999999999999991118 ) ) ;
#17610 = CARTESIAN_POINT ( 'NONE',  ( 3.999999999999997335, -26.16250000000000142, 11.30940107675849404 ) ) ;
#17612 = ORIENTED_EDGE ( 'NONE', *, *, #16025, .T. ) ;
#17611 = CARTESIAN_POINT ( 'NONE',  ( -3.756430356249996549, 25.89062499938548356, 6.831223922626973533 ) ) ;
#17613 = CARTESIAN_POINT ( 'NONE',  ( -1.878215178124998497, 27.80312499938548498, 12.25316411605951927 ) ) ;
#17614 = EDGE_CURVE ( 'NONE', #12311, #21597, #14595, .T. ) ;
#17616 = AXIS2_PLACEMENT_3D ( 'NONE', #4482, #17870, #11852 ) ;
#17615 = CARTESIAN_POINT ( 'NONE',  ( 5.827558883615830965, -30.54913349766226105, 1.000000000000000000 ) ) ;
#17617 = CARTESIAN_POINT ( 'NONE',  ( -24.67207871933484498, 8.377607117416790317, 20.00001200000000523 ) ) ;
#17618 = CARTESIAN_POINT ( 'NONE',  ( 2.000000000000000888, 26.21874999877096712, 12.46410161513774817 ) ) ;
#17619 = VERTEX_POINT ( 'NONE', #16335 ) ;
#17620 = ORIENTED_EDGE ( 'NONE', *, *, #19831, .F. ) ;
#17621 = ADVANCED_FACE ( 'NONE', ( #12272 ), #16588, .T. ) ;
#17622 =( NAMED_UNIT ( * ) SI_UNIT ( $, .STERADIAN. ) SOLID_ANGLE_UNIT ( ) );
#17623 = AXIS2_PLACEMENT_3D ( 'NONE', #16974, #13050, #14621 ) ;
#17624 = CARTESIAN_POINT ( 'NONE',  ( -3.756430356249994329, 29.11562499938548498, 11.16877607737301226 ) ) ;
#17625 = VECTOR ( 'NONE', #15320, 1000.000000000000000 ) ;
#17626 = CARTESIAN_POINT ( 'NONE',  ( 1.878215178125000939, -12.25316411605952283, 0.9656249993854824076 ) ) ;
#17627 = ADVANCED_FACE ( 'NONE', ( #12666 ), #20637, .F. ) ;
#17628 =( BOUNDED_CURVE ( )  B_SPLINE_CURVE ( 2, ( #17572, #8021, #25547, #7633, #8151, #19512, #8410, #4472, #24367 ),
 .UNSPECIFIED., .F., .F. ) 
 B_SPLINE_CURVE_WITH_KNOTS ( ( 3, 2, 2, 2, 3 ),
 ( 0.1749999999999999889, 0.1833333333333333204, 0.2000000000000000111, 0.2166666666666666741, 0.2250000000000000056 ),
 .UNSPECIFIED. ) 
 CURVE ( )  GEOMETRIC_REPRESENTATION_ITEM ( )  RATIONAL_B_SPLINE_CURVE ( ( 0.9330127018922194093, 0.9330127018922194093, 1.000000000000000000, 0.8660254037844387076, 1.000000000000000000, 0.8660254037844387076, 1.000000000000000000, 0.9330127018922194093, 0.9330127018922194093 ) ) 
 REPRESENTATION_ITEM ( '' )  );
#17629 = AXIS2_PLACEMENT_3D ( 'NONE', #22004, #23973, #5926 ) ;
#17630 = DIRECTION ( 'NONE',  ( 0.000000000000000000, 1.000000000000000000, 0.000000000000000000 ) ) ;
#17631 = SURFACE_STYLE_USAGE ( .BOTH. , #1673 ) ;
#17632 = FACE_OUTER_BOUND ( 'NONE', #17776, .T. ) ;
#17633 =( BOUNDED_CURVE ( )  B_SPLINE_CURVE ( 2, ( #9781, #3378, #3761, #15413, #19576, #13322, #17497, #25476, #23386 ),
 .UNSPECIFIED., .F., .F. ) 
 B_SPLINE_CURVE_WITH_KNOTS ( ( 3, 2, 2, 2, 3 ),
 ( 0.07500000000000001110, 0.08333333333333332871, 0.1000000000000000056, 0.1166666666666666685, 0.1250000000000000000 ),
 .UNSPECIFIED. ) 
 CURVE ( )  GEOMETRIC_REPRESENTATION_ITEM ( )  RATIONAL_B_SPLINE_CURVE ( ( 0.9330127018922192983, 0.9330127018922194093, 1.000000000000000000, 0.8660254037844387076, 1.000000000000000000, 0.8660254037844387076, 1.000000000000000000, 0.9330127018922194093, 0.9330127018922194093 ) ) 
 REPRESENTATION_ITEM ( '' )  );
#17634 = CARTESIAN_POINT ( 'NONE',  ( 0.000000000000000000, 0.000000000000000000, 20.00000000000000000 ) ) ;
#17635 = AXIS2_PLACEMENT_3D ( 'NONE', #17904, #11763, #3784 ) ;
#17636 = LINE ( 'NONE', #7308, #20512 ) ;
#17637 = CARTESIAN_POINT ( 'NONE',  ( -1.057460391440397258E-14, 28.71250000000000213, 4.999999999999992006 ) ) ;
#17638 = FACE_OUTER_BOUND ( 'NONE', #7616, .T. ) ;
#17639 = CARTESIAN_POINT ( 'NONE',  ( 3.999999999999994227, -11.30940107675849937, 2.156249998770968457 ) ) ;
#17640 = DIRECTION ( 'NONE',  ( 0.000000000000000000, -0.000000000000000000, 1.000000000000000000 ) ) ;
#17641 = VERTEX_POINT ( 'NONE', #20239 ) ;
#17642 = CARTESIAN_POINT ( 'NONE',  ( -18.28012134629613783, -25.16042852506070560, 1.000000000000000000 ) ) ;
#17643 = CARTESIAN_POINT ( 'NONE',  ( 3.974064950101062088, 29.73565934716929959, 8.475804415688518390 ) ) ;
#17644 = AXIS2_PLACEMENT_3D ( 'NONE', #21545, #1151, #9127 ) ;
#17645 = CARTESIAN_POINT ( 'NONE',  ( 1.878215178125000939, 26.52812499938548285, 12.25316411605952283 ) ) ;
#17646 = AXIS2_PLACEMENT_3D ( 'NONE', #2100, #9936, #12 ) ;
#17647 = CARTESIAN_POINT ( 'NONE',  ( 30.24338421796779386, -7.248980000274303670, 1.000000000000000000 ) ) ;
#17648 = CARTESIAN_POINT ( 'NONE',  ( -3.999999999999997335, 26.55624999877096570, 11.30940107675849404 ) ) ;
#17649 = DIRECTION ( 'NONE',  ( 0.000000000000000000, -0.000000000000000000, 1.000000000000000000 ) ) ;
#17650 = VERTEX_POINT ( 'NONE', #2337 ) ;
#17651 = AXIS2_PLACEMENT_3D ( 'NONE', #85, #22419, #12475 ) ;
#17652 = PLANE ( 'NONE',  #11341 ) ;
#17653 = FACE_OUTER_BOUND ( 'NONE', #21802, .T. ) ;
#17654 = ORIENTED_EDGE ( 'NONE', *, *, #6565, .F. ) ;
#17655 = ORIENTED_EDGE ( 'NONE', *, *, #1970, .F. ) ;
#17656 = EDGE_CURVE ( 'NONE', #10748, #1228, #10600, .T. ) ;
#17657 = EDGE_LOOP ( 'NONE', ( #16378, #18318, #23690, #7352 ) ) ;
#17658 = ORIENTED_EDGE ( 'NONE', *, *, #12460, .T. ) ;
#17659 = PRODUCT_DEFINITION ( 'UNKNOWN', '', #7286, #24842 ) ;
#17660 = VERTEX_POINT ( 'NONE', #13300 ) ;
#17661 = CARTESIAN_POINT ( 'NONE',  ( -16.23990935651735867, -26.52310962334733446, -6.500000000000000000 ) ) ;
#17662 = FACE_OUTER_BOUND ( 'NONE', #16554, .T. ) ;
#17663 = MECHANICAL_DESIGN_GEOMETRIC_PRESENTATION_REPRESENTATION (  '', ( #20584 ), #7629 ) ;
#17664 = DIRECTION ( 'NONE',  ( -0.000000000000000000, -0.000000000000000000, -1.000000000000000000 ) ) ;
#17665 = ADVANCED_FACE ( 'NONE', ( #19174 ), #3222, .T. ) ;
#17666 = DIRECTION ( 'NONE',  ( -0.000000000000000000, -0.000000000000000000, -1.000000000000000000 ) ) ;
#17667 = ADVANCED_FACE ( 'NONE', ( #9255 ), #13053, .F. ) ;
#17668 = CIRCLE ( 'NONE', #20153, 4.000000000000000000 ) ;
#17669 = CARTESIAN_POINT ( 'NONE',  ( 3.756430356250003655, -8.999999999999992895, 3.290624999385483029 ) ) ;
#17670 = CARTESIAN_POINT ( 'NONE',  ( 4.000000000000003553, -6.690598923241489970, 2.681249998770966592 ) ) ;
#17671 = CARTESIAN_POINT ( 'NONE',  ( 3.735045420075836212E-15, 28.51562499938549067, 4.662447845253954171 ) ) ;
#17672 = CARTESIAN_POINT ( 'NONE',  ( -4.000000000000003553, -26.74374999877096926, 8.999999999999992895 ) ) ;
#17673 = DIRECTION ( 'NONE',  ( 0.000000000000000000, 0.000000000000000000, 1.000000000000000000 ) ) ;
#17674 = AXIS2_PLACEMENT_3D ( 'NONE', #17184, #24896, #8810 ) ;
#17675 = CARTESIAN_POINT ( 'NONE',  ( -3.999999999999997335, -11.30940107675849404, 1.612499999999998046 ) ) ;
#17676 = CARTESIAN_POINT ( 'NONE',  ( -4.000000000000003553, -25.84374999877096712, 8.999999999999992895 ) ) ;
#17677 = CARTESIAN_POINT ( 'NONE',  ( -3.999999999999996447, -8.999999999999992895, 2.418749998770966414 ) ) ;
#17678 = CARTESIAN_POINT ( 'NONE',  ( 0.000000000000000000, 0.000000000000000000, -6.500000000000000000 ) ) ;
#17679 = CARTESIAN_POINT ( 'NONE',  ( 3.999999999999997335, -26.55624999877096926, 11.30940107675849404 ) ) ;
#17680 = CARTESIAN_POINT ( 'NONE',  ( 3.756430356250003655, 27.05312499938548498, 8.999999999999992895 ) ) ;
#17681 = DIRECTION ( 'NONE',  ( 0.000000000000000000, 0.000000000000000000, 1.000000000000000000 ) ) ;
#17682 = AXIS2_PLACEMENT_3D ( 'NONE', #9062, #12996, #25635 ) ;
#17683 = LINE ( 'NONE', #6148, #2879 ) ;
#17684 = CARTESIAN_POINT ( 'NONE',  ( -26.75313774936430633, -14.98253926456308172, -6.500000000000000000 ) ) ;
#17685 = EDGE_LOOP ( 'NONE', ( #4849, #5259, #677, #10462 ) ) ;
#17686 = CARTESIAN_POINT ( 'NONE',  ( -1.999999999999998224, 26.95000000000000639, 5.535898384862237620 ) ) ;
#17687 = ORIENTED_EDGE ( 'NONE', *, *, #5241, .T. ) ;
#17688 = VERTEX_POINT ( 'NONE', #8874 ) ;
#17689 = CYLINDRICAL_SURFACE ( 'NONE', #3750, 31.10000000000000142 ) ;
#17690 = ORIENTED_EDGE ( 'NONE', *, *, #5767, .T. ) ;
#17691 = CARTESIAN_POINT ( 'NONE',  ( -1.878215178125004048, -28.02812499938548640, 5.746835883940462963 ) ) ;
#17692 = ORIENTED_EDGE ( 'NONE', *, *, #22750, .T. ) ;
#17693 = CARTESIAN_POINT ( 'NONE',  ( -29.07785765677917311, 9.610428525061202265, -6.500000000000000000 ) ) ;
#17694 = VECTOR ( 'NONE', #25255, 1000.000000000000000 ) ;
#17695 = EDGE_CURVE ( 'NONE', #19787, #12101, #7094, .T. ) ;
#17696 = ORIENTED_EDGE ( 'NONE', *, *, #11851, .T. ) ;
#17697 = CARTESIAN_POINT ( 'NONE',  ( -1.999999999999998224, 26.64999999999999858, 12.46410161513774639 ) ) ;
#17698 = LINE ( 'NONE', #7622, #18917 ) ;
#17699 = ADVANCED_FACE ( 'NONE', ( #8997 ), #10809, .F. ) ;
#17700 =( GEOMETRIC_REPRESENTATION_CONTEXT ( 3 ) GLOBAL_UNCERTAINTY_ASSIGNED_CONTEXT ( ( #25095 ) ) GLOBAL_UNIT_ASSIGNED_CONTEXT ( ( #6131, #23928, #19743 ) ) REPRESENTATION_CONTEXT ( 'NONE', 'WORKASPACE' ) );
#17701 = CARTESIAN_POINT ( 'NONE',  ( -3.756430356249995661, -6.831223922626973533, 0.4406249993854817193 ) ) ;
#17702 = CARTESIAN_POINT ( 'NONE',  ( -1.071796769724485232, 25.58259618943233704, 4.999999999999992006 ) ) ;
#17703 = CARTESIAN_POINT ( 'NONE',  ( 17.29526239452281899, 22.60765715044149715, 11.16877607737301226 ) ) ;
#17704 = DIRECTION ( 'NONE',  ( -0.000000000000000000, -1.000000000000000000, -0.000000000000000000 ) ) ;
#17705 = DIRECTION ( 'NONE',  ( 1.000000000000000000, 0.000000000000000000, -0.000000000000000000 ) ) ;
#17706 = CARTESIAN_POINT ( 'NONE',  ( 2.000000000000000888, 28.52500000000000213, 12.46410161513774817 ) ) ;
#17707 = CARTESIAN_POINT ( 'NONE',  ( 1.878215178125004048, -5.746835883940462963, 0.3281249993854831737 ) ) ;
#17708 = CARTESIAN_POINT ( 'NONE',  ( 23.69483382651587888, 18.38243907059705151, 8.999999999999992895 ) ) ;
#17709 = CARTESIAN_POINT ( 'NONE',  ( -1.071796769724492338, -29.35134618820330488, 12.99999999999999467 ) ) ;
#17710 = ORIENTED_EDGE ( 'NONE', *, *, #105, .F. ) ;
#17711 = ORIENTED_EDGE ( 'NONE', *, *, #10146, .T. ) ;
#17712 = CARTESIAN_POINT ( 'NONE',  ( -3.999999999999994671, 29.70624999877097494, 11.30940107675849404 ) ) ;
#17713 = VERTEX_POINT ( 'NONE', #15152 ) ;
#17714 = CARTESIAN_POINT ( 'NONE',  ( -1.999999999999994893, 29.20000000000000284, 5.535898384862237620 ) ) ;
#17715 = CARTESIAN_POINT ( 'NONE',  ( 18.51293941407127974, 18.51293941407120869, 12.99999999999999112 ) ) ;
#17716 = ORIENTED_EDGE ( 'NONE', *, *, #5464, .F. ) ;
#17717 = ORIENTED_EDGE ( 'NONE', *, *, #18457, .T. ) ;
#17718 = CARTESIAN_POINT ( 'NONE',  ( 1.859271017917182139E-15, 28.88124999877096499, 12.99999999999999289 ) ) ;
#17719 = ORIENTED_EDGE ( 'NONE', *, *, #12171, .T. ) ;
#17720 = CARTESIAN_POINT ( 'NONE',  ( 3.338448572212769694, 38.98643850599027161, 4.611800620969658482 ) ) ;
#17721 = EDGE_CURVE ( 'NONE', #15212, #4479, #3332, .T. ) ;
#17722 = DIRECTION ( 'NONE',  ( 1.000000000000000000, 0.000000000000000000, 0.000000000000000000 ) ) ;
#17723 = CARTESIAN_POINT ( 'NONE',  ( 1.878215178125001605, 27.31562499938548783, 12.25316411605952283 ) ) ;
#17724 = FACE_OUTER_BOUND ( 'NONE', #20199, .T. ) ;
#17725 = CARTESIAN_POINT ( 'NONE',  ( 2.000000000000000000, 27.17500000000000426, 12.46410161513774817 ) ) ;
#17726 = EDGE_CURVE ( 'NONE', #583, #17840, #12516, .T. ) ;
#17727 = CARTESIAN_POINT ( 'NONE',  ( 3.756430356250003655, 25.14062499938548356, 8.999999999999992895 ) ) ;
#17728 = CARTESIAN_POINT ( 'NONE',  ( -1.999999999999995781, -5.535898384862237620, 0.1500000000000008271 ) ) ;
#17729 = EDGE_CURVE ( 'NONE', #5585, #9659, #11075, .T. ) ;
#17730 = CARTESIAN_POINT ( 'NONE',  ( -3.999999999999995559, 27.43750000000000000, 6.690598923241487306 ) ) ;
#17731 = DIRECTION ( 'NONE',  ( 1.000000000000000000, 0.000000000000000000, 0.000000000000000000 ) ) ;
#17732 = CARTESIAN_POINT ( 'NONE',  ( 17.96051224213834985, 20.78893936688446331, 5.535898384862237620 ) ) ;
#17733 = CARTESIAN_POINT ( 'NONE',  ( 22.10384356884614121, 16.79144881292732450, 8.999999999999992895 ) ) ;
#17734 = CARTESIAN_POINT ( 'NONE',  ( -3.213722874945784014, -29.82775332956657266, 11.39306173506716924 ) ) ;
#17735 = CARTESIAN_POINT ( 'NONE',  ( 2.672651547586948120E-15, 29.52812499938548285, 13.33755215474602984 ) ) ;
#17736 = CARTESIAN_POINT ( 'NONE',  ( 21.93836504211864025, 20.46399127338558799, 5.129272290912049392 ) ) ;
#17737 = PLANE ( 'NONE',  #22931 ) ;
#17738 = CARTESIAN_POINT ( 'NONE',  ( 19.42333939484895211, 16.59491227010269299, 5.535898384862238508 ) ) ;
#17739 = ORIENTED_EDGE ( 'NONE', *, *, #20348, .F. ) ;
#17740 = CARTESIAN_POINT ( 'NONE',  ( 2.620986760973688460E-15, 28.43124999877096926, 13.61880215351699874 ) ) ;
#17741 = CARTESIAN_POINT ( 'NONE',  ( -2.620986760973688460E-15, -27.13750000000000284, 13.61880215351699874 ) ) ;
#17743 = ORIENTED_EDGE ( 'NONE', *, *, #3569, .T. ) ;
#17742 = CARTESIAN_POINT ( 'NONE',  ( 3.756430356250002323, 26.11562499938549564, 11.16877607737301403 ) ) ;
#17744 = CARTESIAN_POINT ( 'NONE',  ( 3.756430356250003211, 29.34062499938548640, 6.831223922626973533 ) ) ;
#17745 = ORIENTED_EDGE ( 'NONE', *, *, #13555, .T. ) ;
#17746 = DIRECTION ( 'NONE',  ( 0.000000000000000000, 0.000000000000000000, 1.000000000000000000 ) ) ;
#17747 = VERTEX_POINT ( 'NONE', #7161 ) ;
#17748 = ORIENTED_EDGE ( 'NONE', *, *, #4672, .T. ) ;
#17749 = FACE_OUTER_BOUND ( 'NONE', #18107, .T. ) ;
#17750 = CARTESIAN_POINT ( 'NONE',  ( 3.756430356250004543, 26.00312499938548783, 11.16877607737301226 ) ) ;
#17751 = CARTESIAN_POINT ( 'NONE',  ( 3.756430356250002323, -11.16877607737301403, 3.703124999385482674 ) ) ;
#17752 = ADVANCED_FACE ( 'NONE', ( #12916 ), #19053, .F. ) ;
#17753 = CARTESIAN_POINT ( 'NONE',  ( -1.999999999999995781, 27.34374999877097068, 5.535898384862237620 ) ) ;
#17754 = PRODUCT_CONTEXT ( 'NONE', #19446, 'mechanical' ) ;
#17755 = DIRECTION ( 'NONE',  ( -0.8090169943749417891, 0.5877852522924807976, 0.000000000000000000 ) ) ;
#17756 = EDGE_CURVE ( 'NONE', #24945, #8728, #14959, .T. ) ;
#17757 = CARTESIAN_POINT ( 'NONE',  ( 0.000000000000000000, 0.000000000000000000, 19.50000000000000000 ) ) ;
#17758 = CARTESIAN_POINT ( 'NONE',  ( 15.41874213889414591, 27.00874656207299651, -6.500000000000000000 ) ) ;
#17759 = EDGE_CURVE ( 'NONE', #22817, #25447, #4588, .T. ) ;
#17760 = CARTESIAN_POINT ( 'NONE',  ( -1.999999999999998224, 26.64999999999999858, 12.46410161513774639 ) ) ;
#17761 = CARTESIAN_POINT ( 'NONE',  ( -19.43607991389006528, -24.27856662945486832, -6.500000000000000000 ) ) ;
#17762 = CARTESIAN_POINT ( 'NONE',  ( 19.47643616943617317, 16.82023879147673284, 5.746835883940462963 ) ) ;
#17763 = CARTESIAN_POINT ( 'NONE',  ( 21.12923450446149687, 15.47238025496904612, 6.690598923241489970 ) ) ;
#17764 = VERTEX_POINT ( 'NONE', #5074 ) ;
#17765 = CARTESIAN_POINT ( 'NONE',  ( -5.306793332224213344, 38.77026726007181878, 11.16082596406551986 ) ) ;
#17766 = CARTESIAN_POINT ( 'NONE',  ( 5.239883324427840883, 38.87578012723909637, 6.956022275050601777 ) ) ;
#17767 = CARTESIAN_POINT ( 'NONE',  ( 1.878215178125000939, 28.32812499938548711, 12.25316411605952283 ) ) ;
#17768 = DIRECTION ( 'NONE',  ( 0.8660254037844397068, -0.000000000000000000, 0.4999999999999983347 ) ) ;
#17769 = FACE_OUTER_BOUND ( 'NONE', #16895, .T. ) ;
#17770 = DIRECTION ( 'NONE',  ( 0.000000000000000000, 0.000000000000000000, 1.000000000000000000 ) ) ;
#17771 = ORIENTED_EDGE ( 'NONE', *, *, #10247, .F. ) ;
#17772 = DIRECTION ( 'NONE',  ( -0.7071067811865487940, -0.7071067811865463515, 0.000000000000000000 ) ) ;
#17773 = EDGE_CURVE ( 'NONE', #9386, #7582, #23120, .T. ) ;
#17774 = DIRECTION ( 'NONE',  ( -0.000000000000000000, -0.000000000000000000, 1.000000000000000000 ) ) ;
#17776 = EDGE_LOOP ( 'NONE', ( #8764, #24858, #11109, #9287 ) ) ;
#17775 = CARTESIAN_POINT ( 'NONE',  ( 3.137519842735244810E-15, -26.46249999999999858, 4.999999999999991118 ) ) ;
#17777 = ORIENTED_EDGE ( 'NONE', *, *, #3064, .F. ) ;
#17778 = EDGE_LOOP ( 'NONE', ( #18975, #11020, #2184, #24682 ) ) ;
#17779 = ORIENTED_EDGE ( 'NONE', *, *, #12211, .T. ) ;
#17780 = AXIS2_PLACEMENT_3D ( 'NONE', #6161, #16625, #22896 ) ;
#17781 = EDGE_LOOP ( 'NONE', ( #3424, #13344, #21207, #16722 ) ) ;
#17782 = DIRECTION ( 'NONE',  ( 0.000000000000000000, 0.000000000000000000, -1.000000000000000000 ) ) ;
#17783 =( BOUNDED_CURVE ( )  B_SPLINE_CURVE ( 2, ( #25383, #21340, #2799, #7731, #14845, #10765, #9438 ),
 .UNSPECIFIED., .F., .F. ) 
 B_SPLINE_CURVE_WITH_KNOTS ( ( 3, 2, 2, 3 ),
 ( 0.6000000000000004219, 0.6166666666666670293, 0.6333333333333336368, 0.6500000000000002442 ),
 .UNSPECIFIED. ) 
 CURVE ( )  GEOMETRIC_REPRESENTATION_ITEM ( )  RATIONAL_B_SPLINE_CURVE ( ( 0.9999999999999964473, 0.8660254037844422603, 1.000000000000000000, 0.8660254037844387076, 1.000000000000000000, 0.8660254037844369313, 1.000000000000001776 ) ) 
 REPRESENTATION_ITEM ( '' )  );
#17784 = CARTESIAN_POINT ( 'NONE',  ( -1.626862140677534194E-14, -27.98124999877096997, 12.99999999999999289 ) ) ;
#17785 = CARTESIAN_POINT ( 'NONE',  ( -1.071796769724487230, 26.42634618820330061, 4.999999999999992006 ) ) ;
#17786 = EDGE_CURVE ( 'NONE', #11078, #16594, #19194, .T. ) ;
#17787 = CARTESIAN_POINT ( 'NONE',  ( -2.003086131649545506E-15, 26.37812499938548427, 13.33755215474602984 ) ) ;
#17788 =( BOUNDED_CURVE ( )  B_SPLINE_CURVE ( 2, ( #24061, #4567, #4717, #16491, #4440, #2620, #16607 ),
 .UNSPECIFIED., .F., .F. ) 
 B_SPLINE_CURVE_WITH_KNOTS ( ( 3, 2, 2, 3 ),
 ( 0.09999999999999981126, 0.1166666666666664326, 0.1333333333333330539, 0.1499999999999996891 ),
 .UNSPECIFIED. ) 
 CURVE ( )  GEOMETRIC_REPRESENTATION_ITEM ( )  RATIONAL_B_SPLINE_CURVE ( ( 1.000000000000001776, 0.8660254037844372643, 1.000000000000000000, 0.8660254037844387076, 1.000000000000000000, 0.8660254037844411501, 0.9999999999999975575 ) ) 
 REPRESENTATION_ITEM ( '' )  );
#17789 = CARTESIAN_POINT ( 'NONE',  ( 2.672651547586948120E-15, -13.33755215474602984, 3.628124999385485161 ) ) ;
#17790 = CARTESIAN_POINT ( 'NONE',  ( -1.999999999999998224, -12.46410161513774639, 3.393749998770966503 ) ) ;
#17791 = FILL_AREA_STYLE ('',( #1712 ) ) ;
#17792 = CARTESIAN_POINT ( 'NONE',  ( 2.672651547586948120E-15, 27.39062499938548356, 13.33755215474602984 ) ) ;
#17793 = EDGE_CURVE ( 'NONE', #13062, #1533, #21032, .T. ) ;
#17794 = CARTESIAN_POINT ( 'NONE',  ( 26.49999999999999645, -0.5000000000000000000, 19.50000000000000000 ) ) ;
#17795 = CARTESIAN_POINT ( 'NONE',  ( -0.4995657836784060390, 31.50000000000000000, 14.97916666666665897 ) ) ;
#17796 = CARTESIAN_POINT ( 'NONE',  ( 3.752267015613588906E-15, -4.381197846482986158, 1.912500000000001865 ) ) ;
#17797 = DIRECTION ( 'NONE',  ( -0.000000000000000000, 0.000000000000000000, -1.000000000000000000 ) ) ;
#17798 = CARTESIAN_POINT ( 'NONE',  ( 4.000000000000002665, 26.33124999877097494, 6.690598923241489970 ) ) ;
#17799 = DIRECTION ( 'NONE',  ( 0.000000000000000000, -0.000000000000000000, 1.000000000000000000 ) ) ;
#17800 = EDGE_CURVE ( 'NONE', #2754, #24465, #7536, .T. ) ;
#17801 = CARTESIAN_POINT ( 'NONE',  ( 3.999999999999997335, -27.90624999877097068, 11.30940107675849404 ) ) ;
#17802 = CARTESIAN_POINT ( 'NONE',  ( 3.756430356250004099, 27.99062499938548498, 6.831223922626973533 ) ) ;
#17803 = DIRECTION ( 'NONE',  ( -0.7071067811865487940, -0.7071067811865463515, 0.000000000000000000 ) ) ;
#17804 = FACE_OUTER_BOUND ( 'NONE', #23705, .T. ) ;
#17805 = CYLINDRICAL_SURFACE ( 'NONE', #8891, 0.5000000000000004441 ) ;
#17806 = ORIENTED_EDGE ( 'NONE', *, *, #6265, .F. ) ;
#17807 = ADVANCED_FACE ( 'NONE', ( #15531, #1527 ), #15389, .F. ) ;
#17808 = CARTESIAN_POINT ( 'NONE',  ( 4.000000000000003553, 25.39374999877096784, 8.999999999999992895 ) ) ;
#17809 = ORIENTED_EDGE ( 'NONE', *, *, #2278, .F. ) ;
#17810 = ORIENTED_EDGE ( 'NONE', *, *, #3893, .T. ) ;
#17811 = CARTESIAN_POINT ( 'NONE',  ( 3.878215178125003604, 29.57031249969274356, 8.999999999999992895 ) ) ;
#17812 = ORIENTED_EDGE ( 'NONE', *, *, #18411, .F. ) ;
#17813 = CARTESIAN_POINT ( 'NONE',  ( 1.878215178124998497, -27.80312499938548498, 12.25316411605951927 ) ) ;
#17814 = ORIENTED_EDGE ( 'NONE', *, *, #22691, .F. ) ;
#17815 = CARTESIAN_POINT ( 'NONE',  ( 3.469446951953614189E-15, 40.00000000000000000, 4.999999999999992006 ) ) ;
#17816 = ORIENTED_EDGE ( 'NONE', *, *, #16875, .F. ) ;
#17817 = CARTESIAN_POINT ( 'NONE',  ( -3.999999999999997335, 28.86250000000000071, 11.30940107675849404 ) ) ;
#17818 = LINE ( 'NONE', #13637, #3474 ) ;
#17819 = CARTESIAN_POINT ( 'NONE',  ( -3.756430356249997882, -11.16877607737301226, 0.5156249993854836733 ) ) ;
#17820 = DIRECTION ( 'NONE',  ( -0.8443279255020122998, 0.5358267949790012086, 0.000000000000000000 ) ) ;
#17821 = CARTESIAN_POINT ( 'NONE',  ( 18.86200962215296784, 21.51820700011226606, 5.746835883940462963 ) ) ;
#17822 = CARTESIAN_POINT ( 'NONE',  ( 0.000000000000000000, 0.000000000000000000, 1.000000000000000000 ) ) ;
#17823 = CARTESIAN_POINT ( 'NONE',  ( 20.78010053211970032, 20.78010053211962926, 12.99999999999999289 ) ) ;
#17824 = SHAPE_DEFINITION_REPRESENTATION ( #22165, #23199 ) ;
#17825 = CARTESIAN_POINT ( 'NONE',  ( 3.752267015613588906E-15, 27.36250000000000071, 4.381197846482986158 ) ) ;
#17826 = CARTESIAN_POINT ( 'NONE',  ( 0.000000000000000000, 0.000000000000000000, 1.000000000000000000 ) ) ;
#17827 = CARTESIAN_POINT ( 'NONE',  ( 21.46517399152334704, 18.80897661356389605, 5.746835883940462963 ) ) ;
#17828 = CARTESIAN_POINT ( 'NONE',  ( 8.000000000000000000, 10.00000000000000000, 15.00000000000000178 ) ) ;
#17829 = VERTEX_POINT ( 'NONE', #7794 ) ;
#17830 = EDGE_CURVE ( 'NONE', #14918, #3258, #25050, .T. ) ;
#17831 = ORIENTED_EDGE ( 'NONE', *, *, #3855, .F. ) ;
#17832 = CARTESIAN_POINT ( 'NONE',  ( 3.756430356250002323, 26.11562499938549564, 11.16877607737301226 ) ) ;
#17833 = EDGE_CURVE ( 'NONE', #8878, #89, #7927, .T. ) ;
#17834 = ORIENTED_EDGE ( 'NONE', *, *, #3132, .T. ) ;
#17835 = CARTESIAN_POINT ( 'NONE',  ( -25.75859848311282363, -16.66421332384654974, -6.500000000000000000 ) ) ;
#17836 = CARTESIAN_POINT ( 'NONE',  ( -1.999999999999998224, 29.29374999877096997, 12.46410161513774639 ) ) ;
#17837 = DIRECTION ( 'NONE',  ( 0.000000000000000000, 0.000000000000000000, 1.000000000000000000 ) ) ;
#17838 = CARTESIAN_POINT ( 'NONE',  ( -30.10000000000000142, 3.686186865433532535E-15, 0.000000000000000000 ) ) ;
#17839 = EDGE_LOOP ( 'NONE', ( #10380, #8521, #23405, #8804 ) ) ;
#17840 = VERTEX_POINT ( 'NONE', #23362 ) ;
#17841 = EDGE_CURVE ( 'NONE', #17283, #24856, #23497, .T. ) ;
#17842 = EDGE_CURVE ( 'NONE', #3948, #19738, #25330, .T. ) ;
#17843 = CARTESIAN_POINT ( 'NONE',  ( -3.999999999999999112, 26.03124999877097423, 6.690598923241487306 ) ) ;
#17844 = EDGE_LOOP ( 'NONE', ( #23749, #117, #15328, #25774 ) ) ;
#17845 = DIRECTION ( 'NONE',  ( 0.000000000000000000, 0.000000000000000000, 1.000000000000000000 ) ) ;
#17846 = CARTESIAN_POINT ( 'NONE',  ( -0.5000000000000000000, 0.000000000000000000, 19.50000000000000000 ) ) ;
#17847 = CARTESIAN_POINT ( 'NONE',  ( 3.756430356250003211, 29.19062499938548072, 8.999999999999992895 ) ) ;
#17848 = DIRECTION ( 'NONE',  ( 1.000000000000000000, 0.000000000000000000, 0.000000000000000000 ) ) ;
#17849 = CARTESIAN_POINT ( 'NONE',  ( -1.999999999999998224, 28.00000000000000711, 12.46410161513774639 ) ) ;
#17850 = CARTESIAN_POINT ( 'NONE',  ( -1.878215178124995832, 25.74062499938548498, 5.746835883940462963 ) ) ;
#17851 = DIRECTION ( 'NONE',  ( 1.000000000000000000, 0.000000000000000000, 0.000000000000000000 ) ) ;
#17852 =( BOUNDED_CURVE ( )  B_SPLINE_CURVE ( 2, ( #13130, #20711, #21100, #2790, #22808, #24769, #3178, #12857, #20834 ),
 .UNSPECIFIED., .F., .F. ) 
 B_SPLINE_CURVE_WITH_KNOTS ( ( 3, 2, 2, 2, 3 ),
 ( 0.6250000000000000000, 0.6333333333333333037, 0.6500000000000000222, 0.6666666666666666297, 0.6750000000000000444 ),
 .UNSPECIFIED. ) 
 CURVE ( )  GEOMETRIC_REPRESENTATION_ITEM ( )  RATIONAL_B_SPLINE_CURVE ( ( 0.9330127018922194093, 0.9330127018922194093, 1.000000000000000000, 0.8660254037844387076, 1.000000000000000000, 0.8660254037844387076, 1.000000000000000000, 0.9330127018922189652, 0.9330127018922194093 ) ) 
 REPRESENTATION_ITEM ( '' )  );
#17853 = CYLINDRICAL_SURFACE ( 'NONE', #14707, 26.00000000000000355 ) ;
#17854 = CARTESIAN_POINT ( 'NONE',  ( -16.16421332384646448, 26.25859848311288403, -6.500000000000000000 ) ) ;
#17855 = CARTESIAN_POINT ( 'NONE',  ( 21.48720731330624645, 15.83035306381379748, 6.690598923241489970 ) ) ;
#17856 = CARTESIAN_POINT ( 'NONE',  ( 17.29526239452281899, 22.60765715044149715, 11.16877607737301226 ) ) ;
#17857 = FACE_OUTER_BOUND ( 'NONE', #8662, .T. ) ;
#17858 = CARTESIAN_POINT ( 'NONE',  ( 4.000000000000003553, 28.15000000000000213, 8.999999999999992895 ) ) ;
#17860 = EDGE_CURVE ( 'NONE', #1173, #18977, #11332, .T. ) ;
#17859 = CARTESIAN_POINT ( 'NONE',  ( -3.756430356250003655, -25.59062499938548285, 8.999999999999992895 ) ) ;
#17861 = AXIS2_PLACEMENT_3D ( 'NONE', #25857, #4284, #18272 ) ;
#17862 = CARTESIAN_POINT ( 'NONE',  ( -7.234255490827218082, -30.12293631110037140, 1.000000000000000000 ) ) ;
#17863 = DIRECTION ( 'NONE',  ( 0.000000000000000000, 1.000000000000000000, 0.000000000000000000 ) ) ;
#17864 = ORIENTED_EDGE ( 'NONE', *, *, #15130, .F. ) ;
#17865 = CARTESIAN_POINT ( 'NONE',  ( -3.999999999999997335, 26.55624999877096926, 11.30940107675849404 ) ) ;
#17866 = CARTESIAN_POINT ( 'NONE',  ( -4.000000000000003553, -27.25000000000000000, 8.999999999999992895 ) ) ;
#17868 = VERTEX_POINT ( 'NONE', #1920 ) ;
#17867 = CARTESIAN_POINT ( 'NONE',  ( -1.878215178124996498, 25.85312499938548925, 5.746835883940462963 ) ) ;
#17869 = CARTESIAN_POINT ( 'NONE',  ( 3.756430356250003655, 28.40312499938548640, 8.999999999999992895 ) ) ;
#17870 = DIRECTION ( 'NONE',  ( 0.000000000000000000, 0.000000000000000000, 1.000000000000000000 ) ) ;
#17871 = CARTESIAN_POINT ( 'NONE',  ( 8.377607117416813409, 24.67207871933482366, 20.00001200000000523 ) ) ;
#17872 = CARTESIAN_POINT ( 'NONE',  ( 1.859271017917182139E-15, 29.38750000000000639, 12.99999999999999289 ) ) ;
#17873 = ORIENTED_EDGE ( 'NONE', *, *, #11379, .F. ) ;
#17874 = ORIENTED_EDGE ( 'NONE', *, *, #3174, .T. ) ;
#17875 = CARTESIAN_POINT ( 'NONE',  ( -31.06601413805604039, -1.453535542772269595, -2.750000000000000000 ) ) ;
#17876 = CARTESIAN_POINT ( 'NONE',  ( 3.756430356250004987, 26.49062499938548854, 8.999999999999992895 ) ) ;
#17877 = EDGE_CURVE ( 'NONE', #1168, #12422, #613, .T. ) ;
#17878 = CARTESIAN_POINT ( 'NONE',  ( -1.878215178124995832, -5.746835883940462963, 4.340624999385481964 ) ) ;
#17879 = AXIS2_PLACEMENT_3D ( 'NONE', #24880, #3163, #19109 ) ;
#17880 = CARTESIAN_POINT ( 'NONE',  ( -0.4995657836784084815, 38.49999999999999289, 14.97916666666665897 ) ) ;
#17881 = CARTESIAN_POINT ( 'NONE',  ( 26.00000000000000355, 3.184081677783117796E-15, 20.00001200000000168 ) ) ;
#17882 = DIRECTION ( 'NONE',  ( 0.000000000000000000, -0.000000000000000000, 1.000000000000000000 ) ) ;
#17883 = DIRECTION ( 'NONE',  ( 1.000000000000000000, 0.000000000000000000, -0.000000000000000000 ) ) ;
#17884 = CARTESIAN_POINT ( 'NONE',  ( 18.35384038830430597, 18.35384038830423492, 4.999999999999992006 ) ) ;
#17885 = CYLINDRICAL_SURFACE ( 'NONE', #17082, 4.000000000000000000 ) ;
#17886 = DIRECTION ( 'NONE',  ( 0.000000000000000000, 0.000000000000000000, 1.000000000000000000 ) ) ;
#17887 = CARTESIAN_POINT ( 'NONE',  ( 21.10271800016700183, 15.44586375067455464, 8.999999999999992895 ) ) ;
#17888 = ORIENTED_EDGE ( 'NONE', *, *, #23166, .T. ) ;
#17889 = CARTESIAN_POINT ( 'NONE',  ( -27.10000000000000497, -0.5999999999999998668, 19.59999999999999787 ) ) ;
#17890 = CARTESIAN_POINT ( 'NONE',  ( 3.594806220554922049, 29.78401552627944326, 7.226316032987424975 ) ) ;
#17891 = CARTESIAN_POINT ( 'NONE',  ( 2.672651547586948120E-15, 26.49062499938548143, 13.33755215474602984 ) ) ;
#17892 = CARTESIAN_POINT ( 'NONE',  ( 19.13727975771751488, 17.62153022986539241, 4.999999999999992895 ) ) ;
#17893 = CARTESIAN_POINT ( 'NONE',  ( 3.034965225792634058, 38.86762122992235646, 13.74490037465567127 ) ) ;
#17894 = ORIENTED_EDGE ( 'NONE', *, *, #3425, .F. ) ;
#17895 = CARTESIAN_POINT ( 'NONE',  ( 4.000000000000003553, 27.23124999877096641, 6.690598923241489970 ) ) ;
#17896 = CARTESIAN_POINT ( 'NONE',  ( -5.207925457499139377, 38.94727318402490113, 7.073160566612318512 ) ) ;
#17898 = VERTEX_POINT ( 'NONE', #13565 ) ;
#17897 = DIRECTION ( 'NONE',  ( 0.000000000000000000, 0.000000000000000000, 1.000000000000000000 ) ) ;
#17899 = ORIENTED_EDGE ( 'NONE', *, *, #12424, .T. ) ;
#17901 = EDGE_CURVE ( 'NONE', #5382, #2175, #20292, .T. ) ;
#17900 = ORIENTED_EDGE ( 'NONE', *, *, #18861, .T. ) ;
#17902 = VECTOR ( 'NONE', #10934, 1000.000000000000000 ) ;
#17903 = ORIENTED_EDGE ( 'NONE', *, *, #6083, .T. ) ;
#17904 = CARTESIAN_POINT ( 'NONE',  ( -5.827558883615604479, 30.54913349766230724, -6.500000000000000000 ) ) ;
#17905 = CARTESIAN_POINT ( 'NONE',  ( 3.137519842735244810E-15, -26.91249999999999787, 4.999999999999991118 ) ) ;
#17906 = AXIS2_PLACEMENT_3D ( 'NONE', #9055, #10745, #20824 ) ;
#17907 = CIRCLE ( 'NONE', #14979, 6.000000000000000000 ) ;
#17908 = DIRECTION ( 'NONE',  ( 0.000000000000000000, 0.000000000000000000, 1.000000000000000000 ) ) ;
#17910 = EDGE_CURVE ( 'NONE', #24490, #23177, #5765, .T. ) ;
#17909 = CARTESIAN_POINT ( 'NONE',  ( -1.878215178124999829, 26.34062499938548996, 12.25316411605951927 ) ) ;
#17911 = CARTESIAN_POINT ( 'NONE',  ( 3.756430356250002323, -11.16877607737301226, 1.903124999385483740 ) ) ;
#17912 = CARTESIAN_POINT ( 'NONE',  ( -3.999999999999996447, -8.999999999999992895, 4.668749998770968190 ) ) ;
#17913 = CARTESIAN_POINT ( 'NONE',  ( 3.756430356250004099, 27.99062499938548498, 6.831223922626973533 ) ) ;
#17914 = DIRECTION ( 'NONE',  ( 0.000000000000000000, 0.000000000000000000, 1.000000000000000000 ) ) ;
#17915 = CIRCLE ( 'NONE', #20846, 27.10000000000000142 ) ;
#17916 = CARTESIAN_POINT ( 'NONE',  ( 2.620986760973688460E-15, -13.61880215351699874, 0.7875000000000005329 ) ) ;
#17917 = CARTESIAN_POINT ( 'NONE',  ( -3.999999999999996003, -6.690598923241487306, 2.437499999999999556 ) ) ;
#17918 = AXIS2_PLACEMENT_3D ( 'NONE', #19957, #18751, #7945 ) ;
#17919 = DIRECTION ( 'NONE',  ( -0.000000000000000000, -1.000000000000000000, -0.000000000000000000 ) ) ;
#17920 = CARTESIAN_POINT ( 'NONE',  ( 1.071796769724487230, -25.71115380933864003, 12.99999999999999467 ) ) ;
#17921 = DIRECTION ( 'NONE',  ( 1.000000000000000000, 0.000000000000000000, 0.000000000000000000 ) ) ;
#17922 = CARTESIAN_POINT ( 'NONE',  ( -2.000000000000000888, -28.46874999877097068, 12.46410161513774817 ) ) ;
#17923 = CARTESIAN_POINT ( 'NONE',  ( -3.756430356249996994, 27.27812499938548640, 8.999999999999992895 ) ) ;
#17924 = CARTESIAN_POINT ( 'NONE',  ( 0.000000000000000000, 0.000000000000000000, -6.500000000000000000 ) ) ;
#17926 = CARTESIAN_POINT ( 'NONE',  ( 0.5000000000000001110, 10.00000000000000000, 13.00000000000000178 ) ) ;
#17925 = AXIS2_PLACEMENT_3D ( 'NONE', #14238, #13708, #4295 ) ;
#17927 = DIRECTION ( 'NONE',  ( 0.000000000000000000, 0.000000000000000000, 1.000000000000000000 ) ) ;
#17928 = EDGE_LOOP ( 'NONE', ( #24582, #7199, #23197, #11233 ) ) ;
#17929 = ADVANCED_FACE ( 'NONE', ( #2687 ), #5035, .F. ) ;
#17930 = CARTESIAN_POINT ( 'NONE',  ( -4.000000000000003553, -29.05000000000000071, 8.999999999999992895 ) ) ;
#17932 = VERTEX_POINT ( 'NONE', #8692 ) ;
#17931 = LINE ( 'NONE', #5413, #8320 ) ;
#17933 =( BOUNDED_CURVE ( )  B_SPLINE_CURVE ( 2, ( #6117, #25869, #20107, #21685, #247, #21826, #25738, #8216, #12130 ),
 .UNSPECIFIED., .F., .F. ) 
 B_SPLINE_CURVE_WITH_KNOTS ( ( 3, 2, 2, 2, 3 ),
 ( 0.8250000000000000666, 0.8333333333333333703, 0.8499999999999999778, 0.8666666666666666963, 0.8750000000000000000 ),
 .UNSPECIFIED. ) 
 CURVE ( )  GEOMETRIC_REPRESENTATION_ITEM ( )  RATIONAL_B_SPLINE_CURVE ( ( 0.9330127018922194093, 0.9330127018922198534, 1.000000000000000000, 0.8660254037844387076, 1.000000000000000000, 0.8660254037844387076, 1.000000000000000000, 0.9330127018922194093, 0.9330127018922194093 ) ) 
 REPRESENTATION_ITEM ( '' )  );
#17935 = VERTEX_POINT ( 'NONE', #15114 ) ;
#17934 = EDGE_CURVE ( 'NONE', #2244, #21597, #24983, .T. ) ;
#17936 = CARTESIAN_POINT ( 'NONE',  ( 27.49048467073852464, 14.54246377227360831, 1.000000000000000000 ) ) ;
#17937 = ORIENTED_EDGE ( 'NONE', *, *, #19807, .F. ) ;
#17938 = CARTESIAN_POINT ( 'NONE',  ( -3.756430356250002323, -26.45312499938548356, 11.16877607737301226 ) ) ;
#17939 = EDGE_LOOP ( 'NONE', ( #21615, #9519, #4847, #20991 ) ) ;
#17940 = CARTESIAN_POINT ( 'NONE',  ( -15.41874213889433598, -27.00874656207289704, -6.500000000000000000 ) ) ;
#17941 =( BOUNDED_CURVE ( )  B_SPLINE_CURVE ( 2, ( #16324, #504, #14484, #629, #14999 ),
 .UNSPECIFIED., .F., .F. ) 
 B_SPLINE_CURVE_WITH_KNOTS ( ( 3, 2, 3 ),
 ( 0.9749999999999999778, 0.9833333333333332815, 1.000000000000000000 ),
 .UNSPECIFIED. ) 
 CURVE ( )  GEOMETRIC_REPRESENTATION_ITEM ( )  RATIONAL_B_SPLINE_CURVE ( ( 0.9330127018922194093, 0.9330127018922194093, 1.000000000000000000, 0.8660254037844387076, 1.000000000000000000 ) ) 
 REPRESENTATION_ITEM ( '' )  );
#17942 = AXIS2_PLACEMENT_3D ( 'NONE', #14541, #5686, #1782 ) ;
#17943 = ADVANCED_FACE ( 'NONE', ( #22567 ), #22978, .T. ) ;
#17944 = CIRCLE ( 'NONE', #10392, 0.5000000000000006661 ) ;
#17945 = ORIENTED_EDGE ( 'NONE', *, *, #20164, .F. ) ;
#17946 = EDGE_CURVE ( 'NONE', #3288, #19467, #4928, .T. ) ;
#17947 = CARTESIAN_POINT ( 'NONE',  ( 1.071796769724492338, 29.80134618820330417, 12.99999999999999467 ) ) ;
#17948 = CARTESIAN_POINT ( 'NONE',  ( -3.756430356249996105, 27.24062499938548498, 6.831223922626973533 ) ) ;
#17949 = AXIS2_PLACEMENT_3D ( 'NONE', #6977, #1091, #14957 ) ;
#17950 = AXIS2_PLACEMENT_3D ( 'NONE', #1766, #5549, #9734 ) ;
#17951 = DIRECTION ( 'NONE',  ( 0.000000000000000000, -0.000000000000000000, 1.000000000000000000 ) ) ;
#17952 = CARTESIAN_POINT ( 'NONE',  ( 16.87099832581089132, 22.18339308172956237, 8.999999999999992895 ) ) ;
#17953 = EDGE_CURVE ( 'NONE', #9149, #13257, #11600, .T. ) ;
#17954 = CYLINDRICAL_SURFACE ( 'NONE', #461, 4.000000000000000000 ) ;
#17955 = DIRECTION ( 'NONE',  ( 1.000000000000000000, 0.000000000000000000, 0.000000000000000000 ) ) ;
#17957 = AXIS2_PLACEMENT_3D ( 'NONE', #11789, #19877, #10456 ) ;
#17956 = CONTEXT_DEPENDENT_SHAPE_REPRESENTATION ( #16286, #20722 ) ;
#17958 = CARTESIAN_POINT ( 'NONE',  ( -1.999999999999995781, 28.30000000000000071, 5.535898384862237620 ) ) ;
#17959 = VECTOR ( 'NONE', #1190, 1000.000000000000000 ) ;
#17960 = DIRECTION ( 'NONE',  ( 0.000000000000000000, 0.000000000000000000, -1.000000000000000000 ) ) ;
#17961 = CARTESIAN_POINT ( 'NONE',  ( 18.19682354053567153, 23.50921829645434258, 6.831223922626973533 ) ) ;
#17962 = CARTESIAN_POINT ( 'NONE',  ( -28.34936733434187062, 12.78762572734086866, -6.500000000000000000 ) ) ;
#17963 = ORIENTED_EDGE ( 'NONE', *, *, #12893, .T. ) ;
#17964 = ORIENTED_EDGE ( 'NONE', *, *, #8390, .T. ) ;
#17965 = CARTESIAN_POINT ( 'NONE',  ( 8.012344526598182026E-15, 25.81562499938549138, 4.662447845253954171 ) ) ;
#17966 = ORIENTED_EDGE ( 'NONE', *, *, #25110, .T. ) ;
#17967 = CARTESIAN_POINT ( 'NONE',  ( 4.000000000000001776, 26.31250000000000000, 11.30940107675849760 ) ) ;
#17968 = CARTESIAN_POINT ( 'NONE',  ( 4.000000000000003553, 29.89374999877096784, 8.999999999999992895 ) ) ;
#17969 = APPLICATION_CONTEXT ( 'automotive_design' ) ;
#17970 = CARTESIAN_POINT ( 'NONE',  ( 1.878215178125000939, 29.67812499938548498, 12.25316411605952283 ) ) ;
#17971 = CARTESIAN_POINT ( 'NONE',  ( 19.28502432982091008, 17.76927480196879472, 12.99999999999999112 ) ) ;
#17972 = EDGE_LOOP ( 'NONE', ( #23242, #2343, #11014, #8489 ) ) ;
#17973 = DIRECTION ( 'NONE',  ( 0.000000000000000000, 0.000000000000000000, 1.000000000000000000 ) ) ;
#17974 = AXIS2_PLACEMENT_3D ( 'NONE', #7197, #16890, #25357 ) ;
#17975 = ORIENTED_EDGE ( 'NONE', *, *, #4495, .T. ) ;
#17976 = PRODUCT_DEFINITION ( 'UNKNOWN', '', #4788, #6797 ) ;
#17977 = CARTESIAN_POINT ( 'NONE',  ( 0.07793552093708305817, 39.00000000000049027, 14.49999999999953992 ) ) ;
#17978 = CARTESIAN_POINT ( 'NONE',  ( 3.756430356250004099, 26.07812499938548356, 6.831223922626973533 ) ) ;
#17979 = CARTESIAN_POINT ( 'NONE',  ( 0.000000000000000000, 0.000000000000000000, -6.500000000000000000 ) ) ;
#17980 = AXIS2_PLACEMENT_3D ( 'NONE', #9550, #25261, #15585 ) ;
#17981 = CYLINDRICAL_SURFACE ( 'NONE', #3385, 31.10000000000000142 ) ;
#17982 = DIRECTION ( 'NONE',  ( 0.000000000000000000, 0.000000000000000000, 1.000000000000000000 ) ) ;
#17983 = CARTESIAN_POINT ( 'NONE',  ( -1.999999999999998224, 26.65000000000000568, 12.46410161513774639 ) ) ;
#17984 = ADVANCED_FACE ( 'NONE', ( #20814 ), #2898, .F. ) ;
#17985 = CLOSED_SHELL ( 'NONE', ( #14061, #16207, #1466, #5272, #17312, #22565, #12995, #5050, #19985, #6588, #3938, #2630, #6585, #18181 ) ) ;
#17987 = EDGE_CURVE ( 'NONE', #16614, #15499, #5945, .T. ) ;
#17986 = MECHANICAL_DESIGN_GEOMETRIC_PRESENTATION_REPRESENTATION (  '', ( #15485 ), #4201 ) ;
#17988 = CARTESIAN_POINT ( 'NONE',  ( 1.878215178125004048, 25.66562499938548569, 5.746835883940462963 ) ) ;
#17989 = DIRECTION ( 'NONE',  ( 0.000000000000000000, 0.000000000000000000, 1.000000000000000000 ) ) ;
#17990 = AXIS2_PLACEMENT_3D ( 'NONE', #18115, #6573, #190 ) ;
#17991 = DIRECTION ( 'NONE',  ( 0.4817536741017267032, 0.8763066800438573667, 0.000000000000000000 ) ) ;
#17992 = CARTESIAN_POINT ( 'NONE',  ( 15.61822102945791002, 21.27507527895022221, 6.690598923241487306 ) ) ;
#17993 = PRODUCT_DEFINITION_SHAPE ( 'NONE', 'NONE',  #3722 ) ;
#17994 = CYLINDRICAL_SURFACE ( 'NONE', #21009, 0.5000000000000002220 ) ;
#17995 = CARTESIAN_POINT ( 'NONE',  ( -3.469446951953614189E-15, -30.00000000000000355, 8.999999999999992895 ) ) ;
#17996 = CARTESIAN_POINT ( 'NONE',  ( -1.071796769724493448, 29.12634618820329990, 4.999999999999995559 ) ) ;
#17997 = AXIS2_PLACEMENT_3D ( 'NONE', #8367, #22483, #4180 ) ;
#17998 = CARTESIAN_POINT ( 'NONE',  ( -3.735045420075836212E-15, -26.15312499938548285, 4.662447845253954171 ) ) ;
#17999 = CARTESIAN_POINT ( 'NONE',  ( 19.41885621233737069, 22.07505359029666536, 5.746835883940462963 ) ) ;
#18000 = EDGE_LOOP ( 'NONE', ( #3644, #7059, #7949, #25690 ) ) ;
#18001 = CARTESIAN_POINT ( 'NONE',  ( -3.999999999999997335, 28.35624999877096997, 11.30940107675849404 ) ) ;
#18002 = CARTESIAN_POINT ( 'NONE',  ( 1.999999999999995781, -27.40000000000000213, 5.535898384862237620 ) ) ;
#18004 = ORIENTED_EDGE ( 'NONE', *, *, #19200, .T. ) ;
#18003 = CARTESIAN_POINT ( 'NONE',  ( 4.006172263299091013E-15, 26.71562499938548640, 4.662447845253954171 ) ) ;
#18005 = CIRCLE ( 'NONE', #15504, 0.5000000000000003331 ) ;
#18006 = CARTESIAN_POINT ( 'NONE',  ( -1.878215178124998497, 28.25312499938548427, 12.25316411605951927 ) ) ;
#18007 = AXIS2_PLACEMENT_3D ( 'NONE', #17634, #19573, #9129 ) ;
#18008 = DIRECTION ( 'NONE',  ( 0.000000000000000000, 0.000000000000000000, 1.000000000000000000 ) ) ;
#18009 = CARTESIAN_POINT ( 'NONE',  ( -28.14012133169333651, -13.24173596767349359, 1.000000000000000000 ) ) ;
#18010 = CARTESIAN_POINT ( 'NONE',  ( -1.878215178125000939, -29.56562499938548427, 12.25316411605952283 ) ) ;
#18011 = VERTEX_POINT ( 'NONE', #10865 ) ;
#18012 = ORIENTED_EDGE ( 'NONE', *, *, #21494, .T. ) ;
#18013 = CARTESIAN_POINT ( 'NONE',  ( -3.756430356249996549, 27.61562499938548143, 8.999999999999992895 ) ) ;
#18014 = AXIS2_PLACEMENT_3D ( 'NONE', #1090, #9066, #11276 ) ;
#18015 = ADVANCED_FACE ( 'NONE', ( #16911 ), #4994, .F. ) ;
#18016 = CARTESIAN_POINT ( 'NONE',  ( -1.878215178124998497, -12.25316411605951927, 2.690624999385483385 ) ) ;
#18017 =( BOUNDED_SURFACE ( )  B_SPLINE_SURFACE ( 1, 2, ( 
 ( #24387, #594, #712, #8561, #6586, #12611, #201, #20587, #22023, #2675, #19010, #14958, #22687, #1362, #8816, #4772, #3061, #13252, #1092, #14710, #13134, #6854, #11030, #9068, #17051, #21221, #12744, #16807, #22934, #3305, #2793, #12861, #5019, #24773, #21103, #25022, #7244, #5275, #8957, #3181, #13002, #17190, #1221, #15224, #25162, #20982, #7110, #15096, #14838, #23190, #11278, #24629, #23073, #5158, #11147, #19128, #22812, #19262, #20839, #20713, #16663, #2929, #9200, #18889, #6716, #10758, #18748, #837, #4887, #10890, #976, #16930, #24900, #6978, #1749, #15859, #21876, #21609, #13522, #17703, #3687, #21492, #25671, #23829, #15613, #9455, #7489, #7366, #17821, #25542, #13763, #19780, #21742, #11418, #25786, #11541, #1877, #23449, #7871, #9719, #15478, #5538, #3958, #7751, #17321, #17436, #11667, #13904, #9580, #19507, #3826, #19893, #25402, #5398, #3568, #9839, #1607, #5918, #11924, #13387, #17566 ),
 ( #7626, #23579, #5660, #13640, #19643, #11805, #15734, #23696, #9337, #25284, #5777, #15343, #23312, #21365, #3445, #19391, #1484, #22514, #21997, #4595, #22380, #173, #22122, #22261, #8264, #14421, #16245, #2508, #4073, #8534, #14154, #18214, #14031, #16122, #24216, #6554, #12046, #24084, #295, #10092, #6434, #10335, #18475, #16515, #20160, #4463, #6303, #10474, #12438, #563, #24477, #14296, #4342, #12316, #2127, #14536, #12574, #9961, #430, #20284, #2381, #20406, #8144, #1992, #6166, #15999, #17952, #4208, #18332, #12187, #38, #8399, #16388, #20024, #8014, #23966, #6047, #24354, #18092, #2260, #10216, #1183, #7212, #3033, #15064, #6683, #23039, #5244, #4742, #22901, #18857, #684, #20554, #12715, #8650, #6950, #17153, #4987, #18597, #17023, #10726, #14928, #12967, #20949, #25124, #16629, #20682, #22781, #1066, #2765, #2645, #18982, #9163, #947, #15194, #18712, #8782, #14807, #10607, #9040, #5127 ) ),
 .UNSPECIFIED., .F., .F., .F. ) 
 B_SPLINE_SURFACE_WITH_KNOTS ( ( 2, 2 ),
 ( 3, 2, 2, 2, 2, 2, 2, 2, 2, 2, 2, 2, 2, 2, 2, 2, 2, 2, 2, 2, 2, 2, 2, 2, 2, 2, 2, 2, 2, 2, 2, 2, 2, 2, 2, 2, 2, 2, 2, 2, 2, 2, 2, 2, 2, 2, 2, 2, 2, 2, 2, 2, 2, 2, 2, 2, 2, 2, 2, 2, 3 ),
 ( 0.000000000000000000, 1.000000000000000000 ),
 ( 0.000000000000000000, 0.01666666666666666644, 0.03333333333333333287, 0.05000000000000000278, 0.06666666666666666574, 0.08333333333333332871, 0.1000000000000000056, 0.1166666666666666685, 0.1333333333333333315, 0.1499999999999999944, 0.1666666666666666574, 0.1833333333333333204, 0.2000000000000000111, 0.2166666666666666741, 0.2333333333333333370, 0.2500000000000000000, 0.2666666666666666630, 0.2833333333333333259, 0.2999999999999999889, 0.3166666666666666519, 0.3333333333333333148, 0.3499999999999999778, 0.3666666666666666408, 0.3833333333333333592, 0.4000000000000000222, 0.4166666666666666852, 0.4333333333333333481, 0.4500000000000000111, 0.4666666666666666741, 0.4833333333333333370, 0.5000000000000000000, 0.5166666666666667185, 0.5333333333333333259, 0.5500000000000000444, 0.5666666666666666519, 0.5833333333333333703, 0.5999999999999999778, 0.6166666666666666963, 0.6333333333333333037, 0.6500000000000000222, 0.6666666666666666297, 0.6833333333333333481, 0.6999999999999999556, 0.7166666666666666741, 0.7333333333333332815, 0.7500000000000000000, 0.7666666666666667185, 0.7833333333333333259, 0.8000000000000000444, 0.8166666666666666519, 0.8333333333333333703, 0.8499999999999999778, 0.8666666666666666963, 0.8833333333333333037, 0.9000000000000000222, 0.9166666666666666297, 0.9333333333333333481, 0.9499999999999999556, 0.9666666666666666741, 0.9833333333333332815, 1.000000000000000000 ),
 .UNSPECIFIED. ) 
 GEOMETRIC_REPRESENTATION_ITEM ( )  RATIONAL_B_SPLINE_SURFACE ( (
 ( 1.000000000000000000, 0.8660254037844387076, 1.000000000000000000, 0.8660254037844387076, 1.000000000000000000, 0.8660254037844387076, 1.000000000000000000, 0.8660254037844387076, 1.000000000000000000, 0.8660254037844387076, 1.000000000000000000, 0.8660254037844387076, 1.000000000000000000, 0.8660254037844387076, 1.000000000000000000, 0.8660254037844387076, 1.000000000000000000, 0.8660254037844387076, 1.000000000000000000, 0.8660254037844387076, 1.000000000000000000, 0.8660254037844387076, 1.000000000000000000, 0.8660254037844387076, 1.000000000000000000, 0.8660254037844387076, 1.000000000000000000, 0.8660254037844387076, 1.000000000000000000, 0.8660254037844387076, 1.000000000000000000, 0.8660254037844387076, 1.000000000000000000, 0.8660254037844387076, 1.000000000000000000, 0.8660254037844387076, 1.000000000000000000, 0.8660254037844387076, 1.000000000000000000, 0.8660254037844387076, 1.000000000000000000, 0.8660254037844387076, 1.000000000000000000, 0.8660254037844387076, 1.000000000000000000, 0.8660254037844387076, 1.000000000000000000, 0.8660254037844387076, 1.000000000000000000, 0.8660254037844387076, 1.000000000000000000, 0.8660254037844387076, 1.000000000000000000, 0.8660254037844387076, 1.000000000000000000, 0.8660254037844387076, 1.000000000000000000, 0.8660254037844387076, 1.000000000000000000, 0.8660254037844387076, 1.000000000000000000, 0.8660254037844387076, 1.000000000000000000, 0.8660254037844387076, 1.000000000000000000, 0.8660254037844387076, 1.000000000000000000, 0.8660254037844387076, 1.000000000000000000, 0.8660254037844387076, 1.000000000000000000, 0.8660254037844387076, 1.000000000000000000, 0.8660254037844387076, 1.000000000000000000, 0.8660254037844387076, 1.000000000000000000, 0.8660254037844387076, 1.000000000000000000, 0.8660254037844387076, 1.000000000000000000, 0.8660254037844387076, 1.000000000000000000, 0.8660254037844387076, 1.000000000000000000, 0.8660254037844387076, 1.000000000000000000, 0.8660254037844387076, 1.000000000000000000, 0.8660254037844387076, 1.000000000000000000, 0.8660254037844387076, 1.000000000000000000, 0.8660254037844387076, 1.000000000000000000, 0.8660254037844387076, 1.000000000000000000, 0.8660254037844387076, 1.000000000000000000, 0.8660254037844387076, 1.000000000000000000, 0.8660254037844387076, 1.000000000000000000, 0.8660254037844387076, 1.000000000000000000, 0.8660254037844387076, 1.000000000000000000, 0.8660254037844387076, 1.000000000000000000, 0.8660254037844387076, 1.000000000000000000, 0.8660254037844387076, 1.000000000000000000, 0.8660254037844387076, 1.000000000000000000, 0.8660254037844387076, 1.000000000000000000, 0.8660254037844387076, 1.000000000000000000, 0.8660254037844387076, 1.000000000000000000),
 ( 1.000000000000000000, 0.8660254037844387076, 1.000000000000000000, 0.8660254037844387076, 1.000000000000000000, 0.8660254037844387076, 1.000000000000000000, 0.8660254037844387076, 1.000000000000000000, 0.8660254037844387076, 1.000000000000000000, 0.8660254037844387076, 1.000000000000000000, 0.8660254037844387076, 1.000000000000000000, 0.8660254037844387076, 1.000000000000000000, 0.8660254037844387076, 1.000000000000000000, 0.8660254037844387076, 1.000000000000000000, 0.8660254037844387076, 1.000000000000000000, 0.8660254037844387076, 1.000000000000000000, 0.8660254037844387076, 1.000000000000000000, 0.8660254037844387076, 1.000000000000000000, 0.8660254037844387076, 1.000000000000000000, 0.8660254037844387076, 1.000000000000000000, 0.8660254037844387076, 1.000000000000000000, 0.8660254037844387076, 1.000000000000000000, 0.8660254037844387076, 1.000000000000000000, 0.8660254037844387076, 1.000000000000000000, 0.8660254037844387076, 1.000000000000000000, 0.8660254037844387076, 1.000000000000000000, 0.8660254037844387076, 1.000000000000000000, 0.8660254037844387076, 1.000000000000000000, 0.8660254037844387076, 1.000000000000000000, 0.8660254037844387076, 1.000000000000000000, 0.8660254037844387076, 1.000000000000000000, 0.8660254037844387076, 1.000000000000000000, 0.8660254037844387076, 1.000000000000000000, 0.8660254037844387076, 1.000000000000000000, 0.8660254037844387076, 1.000000000000000000, 0.8660254037844387076, 1.000000000000000000, 0.8660254037844387076, 1.000000000000000000, 0.8660254037844387076, 1.000000000000000000, 0.8660254037844387076, 1.000000000000000000, 0.8660254037844387076, 1.000000000000000000, 0.8660254037844387076, 1.000000000000000000, 0.8660254037844387076, 1.000000000000000000, 0.8660254037844387076, 1.000000000000000000, 0.8660254037844387076, 1.000000000000000000, 0.8660254037844387076, 1.000000000000000000, 0.8660254037844387076, 1.000000000000000000, 0.8660254037844387076, 1.000000000000000000, 0.8660254037844387076, 1.000000000000000000, 0.8660254037844387076, 1.000000000000000000, 0.8660254037844387076, 1.000000000000000000, 0.8660254037844387076, 1.000000000000000000, 0.8660254037844387076, 1.000000000000000000, 0.8660254037844387076, 1.000000000000000000, 0.8660254037844387076, 1.000000000000000000, 0.8660254037844387076, 1.000000000000000000, 0.8660254037844387076, 1.000000000000000000, 0.8660254037844387076, 1.000000000000000000, 0.8660254037844387076, 1.000000000000000000, 0.8660254037844387076, 1.000000000000000000, 0.8660254037844387076, 1.000000000000000000, 0.8660254037844387076, 1.000000000000000000, 0.8660254037844387076, 1.000000000000000000, 0.8660254037844387076, 1.000000000000000000, 0.8660254037844387076, 1.000000000000000000) ) ) 
 REPRESENTATION_ITEM ( '' )  SURFACE ( )  );
#18018 = VECTOR ( 'NONE', #12842, 1000.000000000000000 ) ;
#18019 = ADVANCED_FACE ( 'NONE', ( #11516 ), #11251, .F. ) ;
#18020 = CIRCLE ( 'NONE', #23042, 31.10000000000000142 ) ;
#18021 = DIRECTION ( 'NONE',  ( 0.000000000000000000, 0.000000000000000000, 1.000000000000000000 ) ) ;
#18022 = SURFACE_STYLE_FILL_AREA ( #4277 ) ;
#18023 = DIRECTION ( 'NONE',  ( 1.000000000000000000, 0.000000000000000000, 0.000000000000000000 ) ) ;
#18024 = CIRCLE ( 'NONE', #15929, 31.10000000000000142 ) ;
#18025 = DIRECTION ( 'NONE',  ( -0.1873813145857259888, -0.9822872507286884991, 0.000000000000000000 ) ) ;
#18026 = DIRECTION ( 'NONE',  ( -0.000000000000000000, -0.000000000000000000, 1.000000000000000000 ) ) ;
#18027 = FACE_OUTER_BOUND ( 'NONE', #14764, .T. ) ;
#18028 = CARTESIAN_POINT ( 'NONE',  ( 0.000000000000000000, 0.000000000000000000, -6.500000000000000000 ) ) ;
#18029 = CARTESIAN_POINT ( 'NONE',  ( 16.66113976570983368, 19.31733714366914256, 12.25316411605951927 ) ) ;
#18030 = CARTESIAN_POINT ( 'NONE',  ( 20.74032577480890183, 20.74032577480882722, 13.61880215351699874 ) ) ;
#18031 = VERTEX_POINT ( 'NONE', #21200 ) ;
#18032 = CARTESIAN_POINT ( 'NONE',  ( -5.297276937894413784, 38.97868814324866804, 10.55807547785406797 ) ) ;
#18033 = CARTESIAN_POINT ( 'NONE',  ( 5.357761973269630218, 38.93893882358702285, 7.509353182747807054 ) ) ;
#18034 = CARTESIAN_POINT ( 'NONE',  ( 3.735045420075836212E-15, 27.61562499938548498, 4.662447845253954171 ) ) ;
#18036 = ADVANCED_FACE ( 'NONE', ( #18987 ), #23287, .T. ) ;
#18035 = CARTESIAN_POINT ( 'NONE',  ( -3.471149744654747238, 29.79887180468049479, 6.994934987683496530 ) ) ;
#18037 = CIRCLE ( 'NONE', #3835, 0.5000000000000006661 ) ;
#18038 = LINE ( 'NONE', #123, #23758 ) ;
#18039 = CARTESIAN_POINT ( 'NONE',  ( 3.843461816822868027, 38.61000136877623135, 13.46319918748939948 ) ) ;
#18040 = VERTEX_POINT ( 'NONE', #9046 ) ;
#18041 = CARTESIAN_POINT ( 'NONE',  ( 7.437084071668728555E-15, 26.63124999877097565, 12.99999999999999112 ) ) ;
#18042 = CARTESIAN_POINT ( 'NONE',  ( -30.12293631110050995, -7.734255490826679846, 1.000000000000000000 ) ) ;
#18043 = DIRECTION ( 'NONE',  ( -0.000000000000000000, -0.000000000000000000, 1.000000000000000000 ) ) ;
#18045 = VERTEX_POINT ( 'NONE', #7218 ) ;
#18044 = CARTESIAN_POINT ( 'NONE',  ( 15.67125403804690187, 21.32810828753921228, 11.30940107675849404 ) ) ;
#18046 = AXIS2_PLACEMENT_3D ( 'NONE', #24119, #3726, #15900 ) ;
#18047 = AXIS2_PLACEMENT_3D ( 'NONE', #20165, #6308, #18340 ) ;
#18048 = VERTEX_POINT ( 'NONE', #23046 ) ;
#18049 = ORIENTED_EDGE ( 'NONE', *, *, #15099, .F. ) ;
#18050 = ORIENTED_EDGE ( 'NONE', *, *, #4495, .F. ) ;
#18051 = CARTESIAN_POINT ( 'NONE',  ( 0.000000000000000000, 0.000000000000000000, -6.500000000000000000 ) ) ;
#18053 = DIRECTION ( 'NONE',  ( 0.000000000000000000, 0.000000000000000000, 1.000000000000000000 ) ) ;
#18052 = AXIS2_PLACEMENT_3D ( 'NONE', #6859, #20447, #4496 ) ;
#18054 = ADVANCED_FACE ( 'NONE', ( #13111 ), #13362, .F. ) ;
#18055 = CARTESIAN_POINT ( 'NONE',  ( 3.756430356250002323, 27.80312499938548854, 11.16877607737301226 ) ) ;
#18056 =( BOUNDED_CURVE ( )  B_SPLINE_CURVE ( 2, ( #19278, #24912, #852 ),
 .UNSPECIFIED., .F., .F. ) 
 B_SPLINE_CURVE_WITH_KNOTS ( ( 3, 3 ),
 ( 0.9889400238386636399, 1.000000000000000000 ),
 .UNSPECIFIED. ) 
 CURVE ( )  GEOMETRIC_REPRESENTATION_ITEM ( )  RATIONAL_B_SPLINE_CURVE ( ( 0.9401842259098239785, 0.9110946495778740051, 1.000000000000000000 ) ) 
 REPRESENTATION_ITEM ( '' )  );
#18057 = CARTESIAN_POINT ( 'NONE',  ( 3.756430356250004099, -6.831223922626973533, 4.228124999385484806 ) ) ;
#18058 = CARTESIAN_POINT ( 'NONE',  ( 4.000000000000003553, -8.999999999999992895, 4.443749998770965881 ) ) ;
#18059 = VECTOR ( 'NONE', #3274, 1000.000000000000000 ) ;
#18060 = CARTESIAN_POINT ( 'NONE',  ( 3.756430356250004099, 26.52812499938548285, 6.831223922626973533 ) ) ;
#18061 = EDGE_CURVE ( 'NONE', #1665, #18613, #3158, .T. ) ;
#18062 = AXIS2_PLACEMENT_3D ( 'NONE', #21851, #3933, #7987 ) ;
#18063 = DIRECTION ( 'NONE',  ( -0.000000000000000000, -0.000000000000000000, 1.000000000000000000 ) ) ;
#18064 = CARTESIAN_POINT ( 'NONE',  ( -3.401318489840662096, 30.91344420362552015, -6.500000000000000000 ) ) ;
#18065 = VECTOR ( 'NONE', #10919, 1000.000000000000000 ) ;
#18066 = DIRECTION ( 'NONE',  ( 0.000000000000000000, 0.000000000000000000, 1.000000000000000000 ) ) ;
#18067 = CARTESIAN_POINT ( 'NONE',  ( 9.296355089585910693E-16, 26.18124999877096926, 12.99999999999999289 ) ) ;
#18068 = CARTESIAN_POINT ( 'NONE',  ( 3.878215178125003604, 25.07031249969274356, 8.999999999999992895 ) ) ;
#18069 = CARTESIAN_POINT ( 'NONE',  ( -2.620986760973688460E-15, -28.88124999877096855, 13.61880215351699874 ) ) ;
#18070 = AXIS2_PLACEMENT_3D ( 'NONE', #997, #14860, #16954 ) ;
#18071 = CARTESIAN_POINT ( 'NONE',  ( -1.878215178124995832, 28.55312499938548498, 5.746835883940462963 ) ) ;
#18073 = EDGE_CURVE ( 'NONE', #1503, #8259, #17540, .T. ) ;
#18072 = CARTESIAN_POINT ( 'NONE',  ( 3.834746474454188013E-15, 27.81249999999999645, 4.999999999999992006 ) ) ;
#18074 = CARTESIAN_POINT ( 'NONE',  ( 2.000000000000005329, 28.16874999877097352, 5.535898384862238508 ) ) ;
#18075 = DIRECTION ( 'NONE',  ( 1.000000000000000000, 0.000000000000000000, 0.000000000000000000 ) ) ;
#18076 = ORIENTED_EDGE ( 'NONE', *, *, #9801, .T. ) ;
#18077 = CARTESIAN_POINT ( 'NONE',  ( -1.999999999999998224, 27.10000000000000497, 12.46410161513774639 ) ) ;
#18079 = ORIENTED_EDGE ( 'NONE', *, *, #15311, .F. ) ;
#18078 = DIRECTION ( 'NONE',  ( 0.000000000000000000, 0.000000000000000000, -1.000000000000000000 ) ) ;
#18080=STYLED_ITEM('',(#25900),#4627);
#18081 = ORIENTED_EDGE ( 'NONE', *, *, #21927, .T. ) ;
#18082 = ORIENTED_EDGE ( 'NONE', *, *, #24924, .F. ) ;
#18083 = ORIENTED_EDGE ( 'NONE', *, *, #4824, .T. ) ;
#18084 = ORIENTED_EDGE ( 'NONE', *, *, #13303, .F. ) ;
#18085 = CARTESIAN_POINT ( 'NONE',  ( 4.000000000000003553, 25.39374999877096784, 8.999999999999992895 ) ) ;
#18086 = VECTOR ( 'NONE', #22100, 1000.000000000000000 ) ;
#18087 = VERTEX_POINT ( 'NONE', #5250 ) ;
#18088 = CARTESIAN_POINT ( 'NONE',  ( 4.000000000000003553, 29.08750000000000213, 6.690598923241489970 ) ) ;
#18089 = CARTESIAN_POINT ( 'NONE',  ( 3.735045420075836212E-15, 25.81562499938548783, 4.662447845253954171 ) ) ;
#18090 = CARTESIAN_POINT ( 'NONE',  ( 3.756430356250002323, -11.16877607737301226, 0.6656249993854835845 ) ) ;
#18091 = DIRECTION ( 'NONE',  ( 0.000000000000000000, 0.000000000000000000, 1.000000000000000000 ) ) ;
#18092 = CARTESIAN_POINT ( 'NONE',  ( 17.18919637734483885, 22.50159113326351346, 8.999999999999992895 ) ) ;
#18093 = DIRECTION ( 'NONE',  ( 1.000000000000000000, -0.000000000000000000, 0.000000000000000000 ) ) ;
#18094 = VECTOR ( 'NONE', #9773, 1000.000000000000000 ) ;
#18095 = ADVANCED_FACE ( 'NONE', ( #3543 ), #3414, .F. ) ;
#18096 = CARTESIAN_POINT ( 'NONE',  ( 3.469446951953614189E-15, 35.50000000000000711, 8.999999999999992895 ) ) ;
#18097 = CONTEXT_DEPENDENT_SHAPE_REPRESENTATION ( #10927, #6725 ) ;
#18098 = CARTESIAN_POINT ( 'NONE',  ( 3.756430356250003655, -8.999999999999992895, 1.040624999385484584 ) ) ;
#18099 = CARTESIAN_POINT ( 'NONE',  ( 4.000000000000001776, 27.66249999999999787, 11.30940107675849760 ) ) ;
#18100 = LINE ( 'NONE', #8149, #903 ) ;
#18101 = FACE_OUTER_BOUND ( 'NONE', #8105, .T. ) ;
#18102 = CIRCLE ( 'NONE', #16006, 31.10000000000000142 ) ;
#18103 = EDGE_CURVE ( 'NONE', #15991, #10494, #2019, .T. ) ;
#18104 = CARTESIAN_POINT ( 'NONE',  ( 17.90514199329621903, 23.21753674921489008, 8.999999999999992895 ) ) ;
#18105 = CARTESIAN_POINT ( 'NONE',  ( 0.000000000000000000, 0.000000000000000000, 0.000000000000000000 ) ) ;
#18106 = ORIENTED_EDGE ( 'NONE', *, *, #16972, .F. ) ;
#18107 = EDGE_LOOP ( 'NONE', ( #22608, #25459, #18798, #23303 ) ) ;
#18108 = CARTESIAN_POINT ( 'NONE',  ( 3.756430356250003211, 26.15312499938548996, 8.999999999999992895 ) ) ;
#18109 =( BOUNDED_CURVE ( )  B_SPLINE_CURVE ( 2, ( #11613, #23530, #5613, #25622, #1440, #25741, #9412, #1306, #19588 ),
 .UNSPECIFIED., .F., .F. ) 
 B_SPLINE_CURVE_WITH_KNOTS ( ( 3, 2, 2, 2, 3 ),
 ( 0.3250000000000000111, 0.3333333333333333148, 0.3499999999999999778, 0.3666666666666666408, 0.3750000000000000000 ),
 .UNSPECIFIED. ) 
 CURVE ( )  GEOMETRIC_REPRESENTATION_ITEM ( )  RATIONAL_B_SPLINE_CURVE ( ( 0.9330127018922194093, 0.9330127018922196314, 1.000000000000000000, 0.8660254037844387076, 1.000000000000000000, 0.8660254037844387076, 1.000000000000000000, 0.9330127018922194093, 0.9330127018922194093 ) ) 
 REPRESENTATION_ITEM ( '' )  );
#18110 = ORIENTED_EDGE ( 'NONE', *, *, #12577, .T. ) ;
#18111 = CARTESIAN_POINT ( 'NONE',  ( 0.000000000000000000, 0.000000000000000000, -6.500000000000000000 ) ) ;
#18112 = AXIS2_PLACEMENT_3D ( 'NONE', #14674, #22654, #13103 ) ;
#18113 = CARTESIAN_POINT ( 'NONE',  ( 3.756430356250002323, 26.11562499938548498, 11.16877607737301226 ) ) ;
#18114 = CARTESIAN_POINT ( 'NONE',  ( -1.071796769724492782, 29.18259618943233491, 4.999999999999995559 ) ) ;
#18115 = CARTESIAN_POINT ( 'NONE',  ( 30.12293631110040693, -7.734255490827107948, -6.500000000000000000 ) ) ;
#18116 = ADVANCED_FACE ( 'NONE', ( #1461 ), #11392, .F. ) ;
#18117 = ORIENTED_EDGE ( 'NONE', *, *, #13099, .T. ) ;
#18118 = CIRCLE ( 'NONE', #16868, 4.000000000000000000 ) ;
#18119 = DIRECTION ( 'NONE',  ( 0.000000000000000000, 0.000000000000000000, -1.000000000000000000 ) ) ;
#18120 = ORIENTED_EDGE ( 'NONE', *, *, #20059, .T. ) ;
#18121 = FACE_OUTER_BOUND ( 'NONE', #24943, .T. ) ;
#18122 = CARTESIAN_POINT ( 'NONE',  ( 3.756430356250003655, 27.84062499938548640, 8.999999999999992895 ) ) ;
#18123 = LINE ( 'NONE', #16024, #3847 ) ;
#18124 = DIRECTION ( 'NONE',  ( 0.000000000000000000, 0.000000000000000000, -1.000000000000000000 ) ) ;
#18125 = CARTESIAN_POINT ( 'NONE',  ( 4.000000000000003553, 29.48124999877097352, 6.690598923241489970 ) ) ;
#18126 = EDGE_CURVE ( 'NONE', #7103, #14795, #15586, .T. ) ;
#18127 = CARTESIAN_POINT ( 'NONE',  ( 9.610428525060889626, 29.57785765677927614, -6.500000000000000000 ) ) ;
#18128 = STYLED_ITEM ( 'NONE', ( #16733 ), #3796 ) ;
#18129 = CARTESIAN_POINT ( 'NONE',  ( 3.756430356250003655, 29.64062499938548356, 8.999999999999992895 ) ) ;
#18130 = CARTESIAN_POINT ( 'NONE',  ( 1.626862140677534194E-14, 27.58750000000000213, 12.99999999999999289 ) ) ;
#18131 = AXIS2_PLACEMENT_3D ( 'NONE', #4395, #12497, #24527 ) ;
#18132 = CARTESIAN_POINT ( 'NONE',  ( 17.26224429571663066, 22.91909854520893930, 11.30940107675849404 ) ) ;
#18133 = CARTESIAN_POINT ( 'NONE',  ( 22.32573188046913160, -21.65113613650342472, 1.000000000000000000 ) ) ;
#18134 = ADVANCED_FACE ( 'NONE', ( #17295 ), #23555, .T. ) ;
#18135 = CARTESIAN_POINT ( 'NONE',  ( -1.626862140677534194E-14, -28.43124999877096570, 12.99999999999999289 ) ) ;
#18136 = CARTESIAN_POINT ( 'NONE',  ( 1.071796769724494336, 25.09240381056766367, 4.999999999999992895 ) ) ;
#18137 = CARTESIAN_POINT ( 'NONE',  ( 1.878215178124995832, -25.74062499938548498, 5.746835883940462963 ) ) ;
#18138 = CARTESIAN_POINT ( 'NONE',  ( 26.49999999999999645, 0.5000000000000000000, 19.00000000000000000 ) ) ;
#18139 = ORIENTED_EDGE ( 'NONE', *, *, #18457, .F. ) ;
#18140 = CARTESIAN_POINT ( 'NONE',  ( 2.620986760973688460E-15, 27.08124999877096784, 13.61880215351699874 ) ) ;
#18141 = CARTESIAN_POINT ( 'NONE',  ( -4.000000000000001776, -29.46250000000000568, 11.30940107675849760 ) ) ;
#18142 = EDGE_CURVE ( 'NONE', #23031, #7614, #15071, .T. ) ;
#18144 = ORIENTED_EDGE ( 'NONE', *, *, #9173, .F. ) ;
#18143 = CARTESIAN_POINT ( 'NONE',  ( -1.878215178124999829, 26.45312499938549422, 12.25316411605951927 ) ) ;
#18145 = CARTESIAN_POINT ( 'NONE',  ( 3.756430356250003655, 28.85312499938548569, 8.999999999999992895 ) ) ;
#18146 = EDGE_CURVE ( 'NONE', #22527, #3646, #11127, .T. ) ;
#18147 = DIRECTION ( 'NONE',  ( 1.000000000000000000, 0.000000000000000000, 0.000000000000000000 ) ) ;
#18148 = CARTESIAN_POINT ( 'NONE',  ( -3.999999999999995559, 27.83124999877096784, 6.690598923241487306 ) ) ;
#18149 = VERTEX_POINT ( 'NONE', #25377 ) ;
#18150 = VERTEX_POINT ( 'NONE', #5508 ) ;
#18151 = CARTESIAN_POINT ( 'NONE',  ( -5.706339097770935176, 31.50000000000000000, 7.145898033750358813 ) ) ;
#18152 = CARTESIAN_POINT ( 'NONE',  ( -3.756430356249998326, 28.02812499938548640, 6.831223922626973533 ) ) ;
#18153 = CARTESIAN_POINT ( 'NONE',  ( 3.756430356250002323, -11.16877607737301403, 2.353124999385479477 ) ) ;
#18154 = CARTESIAN_POINT ( 'NONE',  ( -3.137519842735244810E-15, 27.30624999877096926, 4.999999999999991118 ) ) ;
#18155 = CARTESIAN_POINT ( 'NONE',  ( 25.99519186311192342, 0.5000000000000000000, 19.50000000000000000 ) ) ;
#18156 = CARTESIAN_POINT ( 'NONE',  ( 0.000000000000000000, 0.000000000000000000, -6.500000000000000000 ) ) ;
#18157 = CARTESIAN_POINT ( 'NONE',  ( 22.09708691207964293, 16.44023266258718863, 8.999999999999992895 ) ) ;
#18158 = CYLINDRICAL_SURFACE ( 'NONE', #17918, 0.5000000000000004441 ) ;
#18159 = DIRECTION ( 'NONE',  ( -0.000000000000000000, -0.000000000000000000, -1.000000000000000000 ) ) ;
#18160 = CARTESIAN_POINT ( 'NONE',  ( 22.05731215476884088, 16.40045790527639369, 8.999999999999992895 ) ) ;
#18161 = VERTEX_POINT ( 'NONE', #19105 ) ;
#18162 = LINE ( 'NONE', #17889, #2576 ) ;
#18163 = LINE ( 'NONE', #19724, #2129 ) ;
#18164 = AXIS2_PLACEMENT_3D ( 'NONE', #1648, #3484, #11841 ) ;
#18165 = CARTESIAN_POINT ( 'NONE',  ( 1.878215178125000939, 29.22812499938548569, 12.25316411605952283 ) ) ;
#18166 = CARTESIAN_POINT ( 'NONE',  ( -2.004590926901224535, 29.93374515888019971, 5.528701699505815803 ) ) ;
#18167 = LINE ( 'NONE', #4026, #19569 ) ;
#18168 = DIRECTION ( 'NONE',  ( -0.000000000000000000, -0.000000000000000000, 1.000000000000000000 ) ) ;
#18169 = VERTEX_POINT ( 'NONE', #15319 ) ;
#18170 = CARTESIAN_POINT ( 'NONE',  ( 4.000000000000003553, 27.19374999877096855, 8.999999999999992895 ) ) ;
#18171 = CARTESIAN_POINT ( 'NONE',  ( -26.75313774936397948, 14.98253926456367502, 1.000000000000000000 ) ) ;
#18172 = CARTESIAN_POINT ( 'NONE',  ( 1.878215178124995832, -26.64062499938548711, 5.746835883940462963 ) ) ;
#18173 = EDGE_CURVE ( 'NONE', #5321, #18031, #13617, .T. ) ;
#18175 = VERTEX_POINT ( 'NONE', #1581 ) ;
#18174 = CARTESIAN_POINT ( 'NONE',  ( 17.64995053351269405, 19.16570006136466731, 4.999999999999992006 ) ) ;
#18176 = ADVANCED_FACE ( 'NONE', ( #9551 ), #10193, .F. ) ;
#18177 = ORIENTED_EDGE ( 'NONE', *, *, #1798, .T. ) ;
#18178 = ORIENTED_EDGE ( 'NONE', *, *, #18724, .F. ) ;
#18179 = VERTEX_POINT ( 'NONE', #1853 ) ;
#18180 = DIRECTION ( 'NONE',  ( 0.000000000000000000, 0.000000000000000000, 1.000000000000000000 ) ) ;
#18181 = ADVANCED_FACE ( 'NONE', ( #19995 ), #13876, .F. ) ;
#18182 = CARTESIAN_POINT ( 'NONE',  ( -3.756430356249998326, 28.02812499938548640, 6.831223922626973533 ) ) ;
#18183 = CARTESIAN_POINT ( 'NONE',  ( 4.000000000000003553, -6.690598923241489970, 3.581249998770965615 ) ) ;
#18184 = CARTESIAN_POINT ( 'NONE',  ( -1.878215178124995832, 26.64062499938548711, 5.746835883940462963 ) ) ;
#18185 = CARTESIAN_POINT ( 'NONE',  ( -1.952785157361865753, -31.03863125411923463, 1.000000000000000000 ) ) ;
#18186 = CARTESIAN_POINT ( 'NONE',  ( 0.000000000000000000, 0.000000000000000000, 1.000000000000000000 ) ) ;
#18187 = CARTESIAN_POINT ( 'NONE',  ( 3.756430356250003655, 26.49062499938548498, 8.999999999999992895 ) ) ;
#18188 = DIRECTION ( 'NONE',  ( 0.000000000000000000, 0.000000000000000000, 1.000000000000000000 ) ) ;
#18189 = CARTESIAN_POINT ( 'NONE',  ( 3.999999999999997335, -25.65624999877097068, 11.30940107675849404 ) ) ;
#18190 = CARTESIAN_POINT ( 'NONE',  ( 3.401318489841003601, -30.91344420362548107, 1.000000000000000000 ) ) ;
#18191 = CARTESIAN_POINT ( 'NONE',  ( -2.672651547586948120E-15, -25.59062499938548640, 13.33755215474602984 ) ) ;
#18192 = DIRECTION ( 'NONE',  ( 1.000000000000000000, 0.000000000000000000, 0.000000000000000000 ) ) ;
#18193 = CARTESIAN_POINT ( 'NONE',  ( -27.64012133169333651, -13.24173596767349359, -6.500000000000000000 ) ) ;
#18194 = CARTESIAN_POINT ( 'NONE',  ( 2.000000000000000888, -12.46410161513774817, 1.725000000000000755 ) ) ;
#18195 = DIRECTION ( 'NONE',  ( 0.000000000000000000, 0.000000000000000000, 1.000000000000000000 ) ) ;
#18196 = ORIENTED_EDGE ( 'NONE', *, *, #12772, .T. ) ;
#18197 = CARTESIAN_POINT ( 'NONE',  ( -27.25313774936397948, 14.98253926456367502, -6.500000000000000000 ) ) ;
#18199 = ORIENTED_EDGE ( 'NONE', *, *, #1096, .F. ) ;
#18198 = CARTESIAN_POINT ( 'NONE',  ( -2.451530025008688440, 31.00322564728517349, -2.750000000000000000 ) ) ;
#18200 = ADVANCED_FACE ( 'NONE', ( #19756 ), #5891, .T. ) ;
#18201 = EDGE_CURVE ( 'NONE', #5606, #17829, #25656, .T. ) ;
#18202 = ORIENTED_EDGE ( 'NONE', *, *, #8703, .T. ) ;
#18203 = ORIENTED_EDGE ( 'NONE', *, *, #3132, .F. ) ;
#18204 = ORIENTED_EDGE ( 'NONE', *, *, #24600, .T. ) ;
#18205 = ORIENTED_EDGE ( 'NONE', *, *, #6163, .F. ) ;
#18206 = CARTESIAN_POINT ( 'NONE',  ( 25.99519186311192342, 0.5000000000000000000, 19.00000000000000000 ) ) ;
#18207 = EDGE_LOOP ( 'NONE', ( #11558, #19024, #18765, #23685, #15148, #11853, #18177, #5518 ) ) ;
#18208 = AXIS2_PLACEMENT_3D ( 'NONE', #13541, #23714, #13788 ) ;
#18209 = CARTESIAN_POINT ( 'NONE',  ( -3.999999999999997335, 29.31250000000000000, 11.30940107675849404 ) ) ;
#18210 = CARTESIAN_POINT ( 'NONE',  ( 1.878215178125004048, 27.12812499938548783, 5.746835883940462963 ) ) ;
#18211 = EDGE_CURVE ( 'NONE', #14144, #8766, #3264, .T. ) ;
#18212 = CARTESIAN_POINT ( 'NONE',  ( 1.878215178125000939, -12.25316411605952283, 2.428124999385484539 ) ) ;
#18213 = CARTESIAN_POINT ( 'NONE',  ( 9.133673601486252736, -29.72853858738288935, -6.500000000000000000 ) ) ;
#18214 = CARTESIAN_POINT ( 'NONE',  ( 15.94292067550354730, 21.25531543142222901, 11.16877607737301226 ) ) ;
#18215 = FACE_OUTER_BOUND ( 'NONE', #1499, .T. ) ;
#18216 = DIRECTION ( 'NONE',  ( 0.000000000000000000, 0.000000000000000000, 1.000000000000000000 ) ) ;
#18217 = CARTESIAN_POINT ( 'NONE',  ( 1.878215178125004048, -5.746835883940462963, 0.6656249993854841396 ) ) ;
#18218 = LINE ( 'NONE', #17163, #12184 ) ;
#18219 = CARTESIAN_POINT ( 'NONE',  ( -3.756430356249997438, 28.55312499938548498, 11.16877607737301048 ) ) ;
#18220 = LINE ( 'NONE', #7755, #5870 ) ;
#18221 = LINE ( 'NONE', #4960, #25562 ) ;
#18222 = DIRECTION ( 'NONE',  ( -1.000000000000000000, 0.000000000000000000, 0.000000000000000000 ) ) ;
#18223 = EDGE_LOOP ( 'NONE', ( #23539, #5036, #8948, #8029 ) ) ;
#18224 = ORIENTED_EDGE ( 'NONE', *, *, #7762, .T. ) ;
#18225 = CARTESIAN_POINT ( 'NONE',  ( 4.006172263299091013E-15, 27.16562499938548569, 4.662447845253954171 ) ) ;
#18226 = ORIENTED_EDGE ( 'NONE', *, *, #5566, .F. ) ;
#18227 = DIRECTION ( 'NONE',  ( 1.000000000000000000, 0.000000000000000000, 0.000000000000000000 ) ) ;
#18228 = ORIENTED_EDGE ( 'NONE', *, *, #12366, .T. ) ;
#18229 = CARTESIAN_POINT ( 'NONE',  ( 21.39439954740644723, 15.73754529791400181, 11.30940107675849760 ) ) ;
#18230 = EDGE_LOOP ( 'NONE', ( #15241, #13631, #11328, #16112 ) ) ;
#18231 = CYLINDRICAL_SURFACE ( 'NONE', #14025, 4.000000000000000000 ) ;
#18232 = ORIENTED_EDGE ( 'NONE', *, *, #8740, .T. ) ;
#18233 = EDGE_CURVE ( 'NONE', #1729, #14559, #2421, .T. ) ;
#18234 = CARTESIAN_POINT ( 'NONE',  ( -21.28941499438192864, 22.67092431280617859, -6.500000000000000000 ) ) ;
#18235 = CARTESIAN_POINT ( 'NONE',  ( 2.672651547586948120E-15, 26.37812499938548427, 13.33755215474602984 ) ) ;
#18236 = DIRECTION ( 'NONE',  ( 1.000000000000000000, 0.000000000000000000, 0.000000000000000000 ) ) ;
#18237 = AXIS2_PLACEMENT_3D ( 'NONE', #9489, #17472, #19544 ) ;
#18238 = CARTESIAN_POINT ( 'NONE',  ( 28.14012133169314822, -13.24173596767388794, -6.500000000000000000 ) ) ;
#18239 = DIRECTION ( 'NONE',  ( 0.000000000000000000, 0.000000000000000000, 1.000000000000000000 ) ) ;
#18240 = CARTESIAN_POINT ( 'NONE',  ( 3.579383266608310077, 29.78592973091716800, 10.80044967790457378 ) ) ;
#18241 = CARTESIAN_POINT ( 'NONE',  ( 3.756430356250002323, 26.45312499938548356, 11.16877607737301226 ) ) ;
#18242 =( BOUNDED_CURVE ( )  B_SPLINE_CURVE ( 2, ( #3287, #11259, #6151, #21, #17930, #23812, #1730, #21860, #282 ),
 .UNSPECIFIED., .F., .F. ) 
 B_SPLINE_CURVE_WITH_KNOTS ( ( 3, 2, 2, 2, 3 ),
 ( 0.8750000000000000000, 0.8833333333333333037, 0.9000000000000000222, 0.9166666666666666297, 0.9250000000000000444 ),
 .UNSPECIFIED. ) 
 CURVE ( )  GEOMETRIC_REPRESENTATION_ITEM ( )  RATIONAL_B_SPLINE_CURVE ( ( 0.9330127018922194093, 0.9330127018922194093, 1.000000000000000000, 0.8660254037844387076, 1.000000000000000000, 0.8660254037844387076, 1.000000000000000000, 0.9330127018922189652, 0.9330127018922194093 ) ) 
 REPRESENTATION_ITEM ( '' )  );
#18243 = DIRECTION ( 'NONE',  ( 0.000000000000000000, 0.000000000000000000, 1.000000000000000000 ) ) ;
#18244 = CARTESIAN_POINT ( 'NONE',  ( 21.90263254725334363, 19.07420542250708451, 12.46410161513774817 ) ) ;
#18245 = DIRECTION ( 'NONE',  ( 0.1253332335643120576, 0.9921147013144768767, 0.000000000000000000 ) ) ;
#18246 = CARTESIAN_POINT ( 'NONE',  ( -2.000000000000000888, -28.46874999877097068, 12.46410161513774817 ) ) ;
#18247 = CARTESIAN_POINT ( 'NONE',  ( -1.626862140677534194E-14, -27.98124999877096997, 12.99999999999999289 ) ) ;
#18248 = CARTESIAN_POINT ( 'NONE',  ( 3.959305671612554781E-15, 34.00000000000000000, 12.99999999999999289 ) ) ;
#18249 = CARTESIAN_POINT ( 'NONE',  ( 2.000000000000003997, -5.535898384862238508, 1.424999999999999156 ) ) ;
#18250 = ORIENTED_EDGE ( 'NONE', *, *, #113, .T. ) ;
#18251 = CARTESIAN_POINT ( 'NONE',  ( 2.620986760973688460E-15, 26.63124999877097565, 13.61880215351699874 ) ) ;
#18252 = CARTESIAN_POINT ( 'NONE',  ( 0.7500000000000000000, -2.999999999999999556, 17.69999999999999929 ) ) ;
#18254 = ORIENTED_EDGE ( 'NONE', *, *, #741, .F. ) ;
#18253 = CARTESIAN_POINT ( 'NONE',  ( -3.756430356249997882, 28.14062499938548356, 6.831223922626973533 ) ) ;
#18255 = ORIENTED_EDGE ( 'NONE', *, *, #6894, .T. ) ;
#18256 = CARTESIAN_POINT ( 'NONE',  ( 17.87326343783943017, 25.45105997952919097, 1.000000000000000000 ) ) ;
#18257 = CARTESIAN_POINT ( 'NONE',  ( 4.000000000000005329, 27.25000000000000355, 8.999999999999992895 ) ) ;
#18258 = DIRECTION ( 'NONE',  ( -1.000000000000000000, 0.000000000000000000, 0.000000000000000000 ) ) ;
#18259 = ORIENTED_EDGE ( 'NONE', *, *, #20422, .T. ) ;
#18260 = ORIENTED_EDGE ( 'NONE', *, *, #2082, .F. ) ;
#18261 = CARTESIAN_POINT ( 'NONE',  ( -3.735045420075836212E-15, -27.16562499938547859, 4.662447845253954171 ) ) ;
#18262 = CARTESIAN_POINT ( 'NONE',  ( -3.756430356249996105, 27.12812499938548783, 6.831223922626973533 ) ) ;
#18263 = CARTESIAN_POINT ( 'NONE',  ( 3.834746474454188013E-15, 28.20624999877096428, 4.999999999999992006 ) ) ;
#18264 = EDGE_CURVE ( 'NONE', #12515, #130, #13432, .T. ) ;
#18265 = CARTESIAN_POINT ( 'NONE',  ( 4.000000000000005329, 26.38750000000000995, 6.690598923241489970 ) ) ;
#18266 = EDGE_CURVE ( 'NONE', #24375, #23177, #6603, .T. ) ;
#18267 = CARTESIAN_POINT ( 'NONE',  ( -18.28012134629558716, 25.16042852506110705, 1.000000000000000000 ) ) ;
#18268 = ADVANCED_FACE ( 'NONE', ( #8241 ), #12017, .F. ) ;
#18269 = DIRECTION ( 'NONE',  ( 0.000000000000000000, 1.000000000000000000, 0.000000000000000000 ) ) ;
#18270 = DIRECTION ( 'NONE',  ( 0.3090169943749591086, 0.9510565162951497564, 0.000000000000000000 ) ) ;
#18271 = DIRECTION ( 'NONE',  ( -0.7071067811865487940, -0.7071067811865463515, 0.000000000000000000 ) ) ;
#18272 = DIRECTION ( 'NONE',  ( 0.5877852522924853496, 0.8090169943749385695, 0.000000000000000000 ) ) ;
#18273 = CARTESIAN_POINT ( 'NONE',  ( 17.87212389449003425, 23.52897814398233933, 8.999999999999992895 ) ) ;
#18274 = CARTESIAN_POINT ( 'NONE',  ( 18.49305203628493288, 18.49305203628486183, 4.662447845253954171 ) ) ;
#18275 = CARTESIAN_POINT ( 'NONE',  ( 20.26302869750799118, 20.26302869750790947, 4.381197846482986158 ) ) ;
#18276 = EDGE_LOOP ( 'NONE', ( #5548, #24439, #11677, #24437 ) ) ;
#18277 = CARTESIAN_POINT ( 'NONE',  ( 1.071796769724490117, -26.93259618943234202, 4.999999999999992895 ) ) ;
#18278 = DIRECTION ( 'NONE',  ( 0.000000000000000000, 0.000000000000000000, 1.000000000000000000 ) ) ;
#18279 = CARTESIAN_POINT ( 'NONE',  ( 3.756430356250002323, 26.00312499938548427, 11.16877607737301226 ) ) ;
#18281 = ORIENTED_EDGE ( 'NONE', *, *, #4215, .F. ) ;
#18280 = CARTESIAN_POINT ( 'NONE',  ( -2.440392720584789288, 29.90136469312441037, 12.17998752022640296 ) ) ;
#18282 = CARTESIAN_POINT ( 'NONE',  ( 15.25349156384666216, 20.56588631976533676, 6.831223922626973533 ) ) ;
#18283 = CYLINDRICAL_SURFACE ( 'NONE', #15057, 0.5000000000000004441 ) ;
#18284 = VERTEX_POINT ( 'NONE', #9693 ) ;
#18285 = DIRECTION ( 'NONE',  ( 0.000000000000000000, -0.000000000000000000, -1.000000000000000000 ) ) ;
#18286 = DIRECTION ( 'NONE',  ( -0.000000000000000000, -0.000000000000000000, 1.000000000000000000 ) ) ;
#18287 = CARTESIAN_POINT ( 'NONE',  ( 3.756430356249997882, -26.30312499938548498, 11.16877607737301226 ) ) ;
#18289 = ORIENTED_EDGE ( 'NONE', *, *, #14830, .F. ) ;
#18288 = CARTESIAN_POINT ( 'NONE',  ( 18.39361514561510091, 18.39361514561503341, 4.999999999999992006 ) ) ;
#18290 = ORIENTED_EDGE ( 'NONE', *, *, #7331, .F. ) ;
#18291 = EDGE_LOOP ( 'NONE', ( #1563, #10773, #7882, #19579 ) ) ;
#18292 = ORIENTED_EDGE ( 'NONE', *, *, #22216, .T. ) ;
#18293 = CARTESIAN_POINT ( 'NONE',  ( -30.85476721088030061, -3.897863563849544466, 1.000000000000000000 ) ) ;
#18294 = CARTESIAN_POINT ( 'NONE',  ( -1.071796769724490117, 26.87634618820330701, 4.999999999999992895 ) ) ;
#18295 = AXIS2_PLACEMENT_3D ( 'NONE', #6566, #12724, #18222 ) ;
#18296 = FACE_OUTER_BOUND ( 'NONE', #7414, .T. ) ;
#18297 = AXIS2_PLACEMENT_3D ( 'NONE', #6800, #14782, #8368 ) ;
#18298 = CARTESIAN_POINT ( 'NONE',  ( 5.112995299272250684E-15, 27.75624999877097565, 4.999999999999992006 ) ) ;
#18299 = CARTESIAN_POINT ( 'NONE',  ( -1.999999999999998224, -12.46410161513774639, 4.743749998770967480 ) ) ;
#18300 = EDGE_CURVE ( 'NONE', #13208, #25772, #19599, .T. ) ;
#18301 = CARTESIAN_POINT ( 'NONE',  ( 3.756430356250003655, 29.75312499938548783, 8.999999999999992895 ) ) ;
#18302 = EDGE_CURVE ( 'NONE', #8728, #19338, #23276, .T. ) ;
#18303 = CARTESIAN_POINT ( 'NONE',  ( 3.469446951953614189E-15, 30.00000000000000355, 4.999999999999992006 ) ) ;
#18304 = CARTESIAN_POINT ( 'NONE',  ( 3.756430356250003211, 27.42812499938548143, 6.831223922626973533 ) ) ;
#18305 = CARTESIAN_POINT ( 'NONE',  ( 29.09636799667083906, 10.98232076577211558, -6.500000000000000000 ) ) ;
#18306 = CARTESIAN_POINT ( 'NONE',  ( 21.21320343559646915, 21.21320343559638744, 12.99999999999999289 ) ) ;
#18307 = DIRECTION ( 'NONE',  ( -0.3681245526846803617, -0.9297764858882504591, 0.000000000000000000 ) ) ;
#18308 = CARTESIAN_POINT ( 'NONE',  ( 3.999999999999997335, -29.70624999877097139, 11.30940107675849404 ) ) ;
#18309 = EDGE_CURVE ( 'NONE', #9952, #6478, #20802, .T. ) ;
#18310 = DIRECTION ( 'NONE',  ( -0.000000000000000000, -0.000000000000000000, 1.000000000000000000 ) ) ;
#18311 = CARTESIAN_POINT ( 'NONE',  ( 3.752267015613588906E-15, -4.381197846482986158, 2.812499999999997335 ) ) ;
#18312 = AXIS2_PLACEMENT_3D ( 'NONE', #9788, #21305, #3769 ) ;
#18313 = DIRECTION ( 'NONE',  ( 1.000000000000000000, 0.000000000000000000, 0.000000000000000000 ) ) ;
#18314 = DIRECTION ( 'NONE',  ( -0.000000000000000000, -0.000000000000000000, 1.000000000000000000 ) ) ;
#18315 = ORIENTED_EDGE ( 'NONE', *, *, #6789, .F. ) ;
#18316 = CARTESIAN_POINT ( 'NONE',  ( 1.071796769724495446, 27.73615380933864571, 4.999999999999992895 ) ) ;
#18318 = ORIENTED_EDGE ( 'NONE', *, *, #14336, .T. ) ;
#18317 = CARTESIAN_POINT ( 'NONE',  ( 2.000000000000003997, -5.535898384862238508, 3.618749998770966148 ) ) ;
#18319 = ORIENTED_EDGE ( 'NONE', *, *, #12503, .F. ) ;
#18320 = ORIENTED_EDGE ( 'NONE', *, *, #2801, .F. ) ;
#18321 = VERTEX_POINT ( 'NONE', #6658 ) ;
#18322 = ORIENTED_EDGE ( 'NONE', *, *, #13156, .T. ) ;
#18323 = EDGE_LOOP ( 'NONE', ( #6696, #15305, #3910, #13333 ) ) ;
#18324 = CARTESIAN_POINT ( 'NONE',  ( 19.82550637751787548, 19.82550637751778666, 12.99999999999999289 ) ) ;
#18325 = ORIENTED_EDGE ( 'NONE', *, *, #4423, .T. ) ;
#18326 = CARTESIAN_POINT ( 'NONE',  ( 3.063240906311874401, 29.84319947910909931, 11.57226653943512851 ) ) ;
#18327 = CARTESIAN_POINT ( 'NONE',  ( 3.756430356250003655, 27.50312499938548427, 8.999999999999992895 ) ) ;
#18328 = ADVANCED_FACE ( 'NONE', ( #20379 ), #12293, .F. ) ;
#18329 = CARTESIAN_POINT ( 'NONE',  ( 3.735045420075836212E-15, -4.662447845253954171, 3.515624999385486227 ) ) ;
#18330 = VECTOR ( 'NONE', #11984, 1000.000000000000000 ) ;
#18331 = DIRECTION ( 'NONE',  ( 0.000000000000000000, 0.000000000000000000, 1.000000000000000000 ) ) ;
#18332 = CARTESIAN_POINT ( 'NONE',  ( 18.25213002337956780, 20.90832740133887313, 12.25316411605951927 ) ) ;
#18333 = CARTESIAN_POINT ( 'NONE',  ( -24.66042852506064165, 18.28012134629622309, -6.500000000000000000 ) ) ;
#18335 = EDGE_CURVE ( 'NONE', #17313, #1348, #10917, .T. ) ;
#18334 = CIRCLE ( 'NONE', #4114, 31.10000000000000142 ) ;
#18336 = CARTESIAN_POINT ( 'NONE',  ( -4.000000000000003553, -29.69687499938548569, 8.999999999999992895 ) ) ;
#18337 = CIRCLE ( 'NONE', #11645, 4.000000000000000000 ) ;
#18338 = CARTESIAN_POINT ( 'NONE',  ( -3.756430356249997882, -11.16877607737301226, 1.303124999385484095 ) ) ;
#18339 = CARTESIAN_POINT ( 'NONE',  ( -3.999999999999997335, -11.30940107675849404, 3.412499999999996980 ) ) ;
#18340 = DIRECTION ( 'NONE',  ( 1.000000000000000000, 0.000000000000000000, 0.000000000000000000 ) ) ;
#18341 = CARTESIAN_POINT ( 'NONE',  ( 20.20656826142266738, -23.64116323484245541, -6.500000000000000000 ) ) ;
#18342 = CARTESIAN_POINT ( 'NONE',  ( -3.756430356249996105, -6.831223922626973533, 2.690624999385480276 ) ) ;
#18343 = CARTESIAN_POINT ( 'NONE',  ( 27.92360179968372691, -13.69242354489151836, 1.000000000000000000 ) ) ;
#18344 = FACE_OUTER_BOUND ( 'NONE', #12822, .T. ) ;
#18345 = ORIENTED_EDGE ( 'NONE', *, *, #3890, .T. ) ;
#18346 = ORIENTED_EDGE ( 'NONE', *, *, #8900, .T. ) ;
#18347 = CARTESIAN_POINT ( 'NONE',  ( -3.756430356249998326, 28.14062499938548356, 6.831223922626973533 ) ) ;
#18348 = ADVANCED_FACE ( 'NONE', ( #4317 ), #10447, .F. ) ;
#18350 = VERTEX_POINT ( 'NONE', #8898 ) ;
#18349 = CIRCLE ( 'NONE', #7070, 24.00000000000000355 ) ;
#18351 = DIRECTION ( 'NONE',  ( -0.000000000000000000, -1.000000000000000000, -0.000000000000000000 ) ) ;
#18352 = ORIENTED_EDGE ( 'NONE', *, *, #20348, .T. ) ;
#18353 = VERTEX_POINT ( 'NONE', #12689 ) ;
#18354 = AXIS2_PLACEMENT_3D ( 'NONE', #6433, #24215, #1991 ) ;
#18355 = DIRECTION ( 'NONE',  ( 1.000000000000000000, -0.000000000000000000, -0.000000000000000000 ) ) ;
#18356 = CIRCLE ( 'NONE', #12947, 31.10000000000000142 ) ;
#18357 = VERTEX_POINT ( 'NONE', #2619 ) ;
#18358 = DIRECTION ( 'NONE',  ( 1.000000000000000000, 0.000000000000000000, 0.000000000000000000 ) ) ;
#18359 = CARTESIAN_POINT ( 'NONE',  ( 3.756430356250003655, 27.39062499938548356, 8.999999999999992895 ) ) ;
#18360 = CARTESIAN_POINT ( 'NONE',  ( 3.469446951953614189E-15, 34.00000000000000000, 8.999999999999992895 ) ) ;
#18361 = VECTOR ( 'NONE', #23297, 1000.000000000000000 ) ;
#18362 = DIRECTION ( 'NONE',  ( -0.000000000000000000, -0.000000000000000000, -1.000000000000000000 ) ) ;
#18363 = CARTESIAN_POINT ( 'NONE',  ( 2.003086131649545506E-15, 29.38750000000000284, 13.61880215351699874 ) ) ;
#18364 = CIRCLE ( 'NONE', #22550, 0.4999999999999993894 ) ;
#18365 = VECTOR ( 'NONE', #3110, 1000.000000000000000 ) ;
#18366 = CARTESIAN_POINT ( 'NONE',  ( 1.878215178125000939, 28.66562499938548569, 12.25316411605952283 ) ) ;
#18367 = EDGE_CURVE ( 'NONE', #4477, #5974, #1596, .T. ) ;
#18368 = CARTESIAN_POINT ( 'NONE',  ( -7.248980000273892443, 30.24338421796789333, 1.000000000000000000 ) ) ;
#18369 = AXIS2_PLACEMENT_3D ( 'NONE', #18998, #9324, #7353 ) ;
#18370 = CARTESIAN_POINT ( 'NONE',  ( -0.4451413195715977489, 38.71736240459208034, 3.234498339501550745 ) ) ;
#18371 = DIRECTION ( 'NONE',  ( 0.000000000000000000, 0.000000000000000000, 1.000000000000000000 ) ) ;
#18372 = CARTESIAN_POINT ( 'NONE',  ( 1.999999999999998224, -27.94374999877096855, 12.46410161513774639 ) ) ;
#18373 = CARTESIAN_POINT ( 'NONE',  ( 1.878215178124998497, -25.44062499938548427, 12.25316411605951927 ) ) ;
#18374 = CARTESIAN_POINT ( 'NONE',  ( 5.396012270207167560, 38.91143067427094593, 10.45569860586814137 ) ) ;
#18375 = VECTOR ( 'NONE', #3014, 1000.000000000000000 ) ;
#18376 = ORIENTED_EDGE ( 'NONE', *, *, #1122, .F. ) ;
#18377 = CARTESIAN_POINT ( 'NONE',  ( 3.756430356250002323, 25.66562499938548569, 11.16877607737301226 ) ) ;
#18378 = CARTESIAN_POINT ( 'NONE',  ( 1.999999999999998224, -28.00000000000000000, 12.46410161513774639 ) ) ;
#18380 = ORIENTED_EDGE ( 'NONE', *, *, #9920, .F. ) ;
#18379 = CARTESIAN_POINT ( 'NONE',  ( 1.878215178125005158, 28.47812499938549280, 5.746835883940462963 ) ) ;
#18381 = ORIENTED_EDGE ( 'NONE', *, *, #5227, .T. ) ;
#18382 = DIRECTION ( 'NONE',  ( 0.000000000000000000, -0.000000000000000000, 1.000000000000000000 ) ) ;
#18383 = AXIS2_PLACEMENT_3D ( 'NONE', #22786, #4862, #3038 ) ;
#18384 = CIRCLE ( 'NONE', #8359, 4.000000000000000000 ) ;
#18385 = CARTESIAN_POINT ( 'NONE',  ( 3.469446951953614189E-15, -8.999999999999992895, 6.000000000000000000 ) ) ;
#18386 = CARTESIAN_POINT ( 'NONE',  ( 27.00874656207300717, -15.41874213889412815, 1.000000000000000000 ) ) ;
#18387 = VERTEX_POINT ( 'NONE', #16880 ) ;
#18388 = ORIENTED_EDGE ( 'NONE', *, *, #3162, .F. ) ;
#18389 = CARTESIAN_POINT ( 'NONE',  ( 3.756430356249997438, -26.41562499938548569, 11.16877607737301048 ) ) ;
#18390 = CARTESIAN_POINT ( 'NONE',  ( -1.878215178124996498, 27.54062499938548569, 5.746835883940462963 ) ) ;
#18391 = CARTESIAN_POINT ( 'NONE',  ( -27.10000000000000497, 0.6000000000000000888, 19.00000000000000000 ) ) ;
#18392 = FACE_OUTER_BOUND ( 'NONE', #14974, .T. ) ;
#18393 = AXIS2_PLACEMENT_3D ( 'NONE', #2267, #21751, #22132 ) ;
#18394 = CARTESIAN_POINT ( 'NONE',  ( 20.58122674904192451, 20.58122674904186411, 4.999999999999992006 ) ) ;
#18395 = DIRECTION ( 'NONE',  ( 0.000000000000000000, -1.000000000000000000, 0.000000000000000000 ) ) ;
#18396 = CARTESIAN_POINT ( 'NONE',  ( 3.959305671612554781E-15, 25.00000000000000000, 12.99999999999999289 ) ) ;
#18397 = VECTOR ( 'NONE', #5470, 1000.000000000000000 ) ;
#18398 = AXIS2_PLACEMENT_3D ( 'NONE', #3688, #5920, #18093 ) ;
#18399 = CARTESIAN_POINT ( 'NONE',  ( -24.27856662945480437, 19.43607991389013989, -2.750000000000000000 ) ) ;
#18400 = EDGE_CURVE ( 'NONE', #19344, #3259, #12448, .T. ) ;
#18401 = CARTESIAN_POINT ( 'NONE',  ( 24.00000000000000355, 0.000000000000000000, 17.00000000000000000 ) ) ;
#18402 = DIRECTION ( 'NONE',  ( 0.000000000000000000, 0.000000000000000000, 1.000000000000000000 ) ) ;
#18403 = CARTESIAN_POINT ( 'NONE',  ( 19.76584424242071947, 19.76584424242064486, 4.662447845253954171 ) ) ;
#18404 = CARTESIAN_POINT ( 'NONE',  ( 17.83234913717923220, 23.48920338667153729, 8.999999999999992895 ) ) ;
#18405 = CARTESIAN_POINT ( 'NONE',  ( -3.999999999999996447, 28.37500000000000000, 8.999999999999992895 ) ) ;
#18406 = LINE ( 'NONE', #12512, #17585 ) ;
#18407 = CARTESIAN_POINT ( 'NONE',  ( -3.756430356249995661, 26.22812499938548214, 6.831223922626973533 ) ) ;
#18408 = AXIS2_PLACEMENT_3D ( 'NONE', #8747, #12684, #16602 ) ;
#18411 = EDGE_CURVE ( 'NONE', #25359, #6673, #12033, .T. ) ;
#18410 = EDGE_LOOP ( 'NONE', ( #12554, #10330, #18250, #21450 ) ) ;
#18409 = CARTESIAN_POINT ( 'NONE',  ( -3.999903055931597784, 29.73215053696358368, 8.737301635141733414 ) ) ;
#18412 = DIRECTION ( 'NONE',  ( 0.000000000000000000, 1.000000000000000000, 0.000000000000000000 ) ) ;
#18413 = CARTESIAN_POINT ( 'NONE',  ( 3.999999999999997335, -27.96250000000000213, 11.30940107675849404 ) ) ;
#18414 = EDGE_LOOP ( 'NONE', ( #9058, #13476, #22342, #16018 ) ) ;
#18415 = DIRECTION ( 'NONE',  ( 1.000000000000000000, 0.000000000000000000, 0.000000000000000000 ) ) ;
#18416 = DIRECTION ( 'NONE',  ( 0.000000000000000000, 1.000000000000000000, 0.000000000000000000 ) ) ;
#18417 = CARTESIAN_POINT ( 'NONE',  ( -1.878215178125004048, -27.01562499938548711, 5.746835883940462963 ) ) ;
#18419 = ORIENTED_EDGE ( 'NONE', *, *, #1174, .T. ) ;
#18418 = CARTESIAN_POINT ( 'NONE',  ( 18.55271417138208179, 18.55271417138200363, 12.99999999999999112 ) ) ;
#18420 = EDGE_CURVE ( 'NONE', #17283, #18643, #9949, .T. ) ;
#18421 = DIRECTION ( 'NONE',  ( 0.000000000000000000, 0.000000000000000000, -1.000000000000000000 ) ) ;
#18422 = ORIENTED_EDGE ( 'NONE', *, *, #20875, .F. ) ;
#18423 = CARTESIAN_POINT ( 'NONE',  ( 3.756430356249996994, -29.52812499938548640, 8.999999999999992895 ) ) ;
#18424 = ORIENTED_EDGE ( 'NONE', *, *, #16544, .T. ) ;
#18425 = PRODUCT ( 'revolution counter', 'revolution counter', '', ( #9842 ) ) ;
#18426 = EDGE_CURVE ( 'NONE', #19882, #5382, #12412, .T. ) ;
#18427 = ORIENTED_EDGE ( 'NONE', *, *, #6840, .F. ) ;
#18428 = CARTESIAN_POINT ( 'NONE',  ( 13.69242354489133895, -27.92360179968382283, 1.000000000000000000 ) ) ;
#18429 = VECTOR ( 'NONE', #25320, 1000.000000000000000 ) ;
#18430 = CARTESIAN_POINT ( 'NONE',  ( -3.918623196469422698, 38.49999999999999289, 13.54361004533748059 ) ) ;
#18431 = CIRCLE ( 'NONE', #9238, 31.10000000000000142 ) ;
#18432 = CARTESIAN_POINT ( 'NONE',  ( -25.99307600111999150, -0.5999999999999996447, 19.59999999999999787 ) ) ;
#18433 = CIRCLE ( 'NONE', #1732, 0.5000000000000001110 ) ;
#18434 = CARTESIAN_POINT ( 'NONE',  ( -3.756430356249996994, -8.999999999999992895, 3.178124999385484983 ) ) ;
#18435 = DIRECTION ( 'NONE',  ( -0.7071067811865487940, -0.7071067811865463515, 0.000000000000000000 ) ) ;
#18436 = CARTESIAN_POINT ( 'NONE',  ( 2.672651547586948120E-15, 29.64062499938548356, 13.33755215474602984 ) ) ;
#18437 = DIRECTION ( 'NONE',  ( 0.000000000000000000, 0.000000000000000000, 1.000000000000000000 ) ) ;
#18438 = AXIS2_PLACEMENT_3D ( 'NONE', #3443, #15221, #3179 ) ;
#18439 = CARTESIAN_POINT ( 'NONE',  ( 0.000000000000000000, 0.000000000000000000, -6.500000000000000000 ) ) ;
#18440 = CARTESIAN_POINT ( 'NONE',  ( -3.756430356249996105, 26.22812499938548214, 6.831223922626973533 ) ) ;
#18441 = CARTESIAN_POINT ( 'NONE',  ( -25.98730014090418194, 17.08421000182805471, -2.750000000000000000 ) ) ;
#18442 = DIRECTION ( 'NONE',  ( -0.8660254037844395958, -0.4999999999999982792, 0.000000000000000000 ) ) ;
#18443 = CARTESIAN_POINT ( 'NONE',  ( -8.831537335106614961E-15, -26.23749999999999716, 12.99999999999999112 ) ) ;
#18444 = CARTESIAN_POINT ( 'NONE',  ( 1.999999999999998224, -28.84374999877096712, 12.46410161513774639 ) ) ;
#18445 = AXIS2_PLACEMENT_3D ( 'NONE', #5693, #13805, #22031 ) ;
#18446 = CARTESIAN_POINT ( 'NONE',  ( -1.878215178124995832, 29.45312499938548356, 5.746835883940462963 ) ) ;
#18447 = VECTOR ( 'NONE', #10221, 1000.000000000000000 ) ;
#18448 = CARTESIAN_POINT ( 'NONE',  ( -28.91604871112473418, -11.44867358849319849, 1.000000000000000000 ) ) ;
#18449 = EDGE_CURVE ( 'NONE', #1143, #12917, #24559, .T. ) ;
#18450 = CARTESIAN_POINT ( 'NONE',  ( 1.071796769724487230, -25.31740381056767220, 12.99999999999999467 ) ) ;
#18451 = CARTESIAN_POINT ( 'NONE',  ( -12.74173596767398742, -28.14012133169310559, -6.500000000000000000 ) ) ;
#18452 = ORIENTED_EDGE ( 'NONE', *, *, #1178, .T. ) ;
#18453 = VECTOR ( 'NONE', #23859, 1000.000000000000000 ) ;
#18454 = CARTESIAN_POINT ( 'NONE',  ( 3.756430356250003655, 25.19687499938548569, 8.999999999999992895 ) ) ;
#18456 = ORIENTED_EDGE ( 'NONE', *, *, #10643, .F. ) ;
#18455 = CARTESIAN_POINT ( 'NONE',  ( 5.112995299272250684E-15, 26.01250000000000284, 4.999999999999992006 ) ) ;
#18457 = EDGE_CURVE ( 'NONE', #7884, #23296, #24132, .T. ) ;
#18458 = AXIS2_PLACEMENT_3D ( 'NONE', #17642, #14232, #16068 ) ;
#18459 = ORIENTED_EDGE ( 'NONE', *, *, #8853, .F. ) ;
#18460 = VERTEX_POINT ( 'NONE', #18576 ) ;
#18461 = ORIENTED_EDGE ( 'NONE', *, *, #6227, .F. ) ;
#18462 = ADVANCED_FACE ( 'NONE', ( #14513 ), #22484, .T. ) ;
#18463 = EDGE_LOOP ( 'NONE', ( #15718, #8257, #25008, #7025, #20700 ) ) ;
#18464 = ORIENTED_EDGE ( 'NONE', *, *, #16284, .T. ) ;
#18465 = FACE_OUTER_BOUND ( 'NONE', #20073, .T. ) ;
#18466 = EDGE_CURVE ( 'NONE', #24513, #11524, #14646, .T. ) ;
#18467 = AXIS2_PLACEMENT_3D ( 'NONE', #24619, #6846, #1086 ) ;
#18468 = ORIENTED_EDGE ( 'NONE', *, *, #15311, .T. ) ;
#18469 = DIRECTION ( 'NONE',  ( 0.000000000000000000, 0.000000000000000000, 1.000000000000000000 ) ) ;
#18470 = CARTESIAN_POINT ( 'NONE',  ( 1.878215178125004048, 26.22812499938548569, 5.746835883940462963 ) ) ;
#18471 = VECTOR ( 'NONE', #14506, 1000.000000000000000 ) ;
#18472 = CIRCLE ( 'NONE', #14713, 0.5000000000000002220 ) ;
#18473 = CARTESIAN_POINT ( 'NONE',  ( 3.756430356250003655, -8.999999999999992895, 2.053124999385484095 ) ) ;
#18474 = SURFACE_SIDE_STYLE ('',( #4462 ) ) ;
#18475 = CARTESIAN_POINT ( 'NONE',  ( 16.23460222274299980, 21.54699697866167440, 8.999999999999992895 ) ) ;
#18476 =( BOUNDED_CURVE ( )  B_SPLINE_CURVE ( 2, ( #4274, #20611, #16447, #16054, #16172, #10391, #12639, #8319, #18263 ),
 .UNSPECIFIED., .F., .F. ) 
 B_SPLINE_CURVE_WITH_KNOTS ( ( 3, 2, 2, 2, 3 ),
 ( 0.5750000000000000666, 0.5833333333333333703, 0.5999999999999999778, 0.6166666666666666963, 0.6250000000000000000 ),
 .UNSPECIFIED. ) 
 CURVE ( )  GEOMETRIC_REPRESENTATION_ITEM ( )  RATIONAL_B_SPLINE_CURVE ( ( 0.9330127018922194093, 0.9330127018922198534, 1.000000000000000000, 0.8660254037844387076, 1.000000000000000000, 0.8660254037844387076, 1.000000000000000000, 0.9330127018922194093, 0.9330127018922194093 ) ) 
 REPRESENTATION_ITEM ( '' )  );
#18477 = CARTESIAN_POINT ( 'NONE',  ( 20.30280345481879323, 20.30280345481869730, 4.999999999999992006 ) ) ;
#18478 = DIRECTION ( 'NONE',  ( -0.000000000000000000, -1.000000000000000000, -0.000000000000000000 ) ) ;
#18479 = CARTESIAN_POINT ( 'NONE',  ( 3.735045420075836212E-15, -4.662447845253954171, 2.053124999385483207 ) ) ;
#18480 = SURFACE_STYLE_FILL_AREA ( #9992 ) ;
#18481 = DIRECTION ( 'NONE',  ( 0.000000000000000000, 0.000000000000000000, 1.000000000000000000 ) ) ;
#18482 = CARTESIAN_POINT ( 'NONE',  ( 3.469446951953614189E-15, 40.00000000000000000, 4.999999999999992006 ) ) ;
#18483 = CARTESIAN_POINT ( 'NONE',  ( 2.672651547586948120E-15, 28.17812499938548143, 13.33755215474603162 ) ) ;
#18484 =( BOUNDED_CURVE ( )  B_SPLINE_CURVE ( 2, ( #2389, #24226, #6694, #24609, #8659 ),
 .UNSPECIFIED., .F., .F. ) 
 B_SPLINE_CURVE_WITH_KNOTS ( ( 3, 2, 3 ),
 ( 0.000000000000000000, 0.01666666666666666644, 0.02500000000000000486 ),
 .UNSPECIFIED. ) 
 CURVE ( )  GEOMETRIC_REPRESENTATION_ITEM ( )  RATIONAL_B_SPLINE_CURVE ( ( 1.000000000000000000, 0.8660254037844387076, 1.000000000000000000, 0.9330127018922192983, 0.9330127018922194093 ) ) 
 REPRESENTATION_ITEM ( '' )  );
#18485 = CARTESIAN_POINT ( 'NONE',  ( -3.756430356249997438, -11.16877607737301048, 1.415624999385483029 ) ) ;
#18486 = DIRECTION ( 'NONE',  ( -0.7071067811865487940, -0.7071067811865463515, 0.000000000000000000 ) ) ;
#18487 = CIRCLE ( 'NONE', #19716, 31.10000000000000142 ) ;
#18488 = ORIENTED_EDGE ( 'NONE', *, *, #12668, .T. ) ;
#18489 = ORIENTED_EDGE ( 'NONE', *, *, #23797, .F. ) ;
#18490 = CARTESIAN_POINT ( 'NONE',  ( -1.878215178124996498, 27.20312499938549067, 5.746835883940462963 ) ) ;
#18491 = AXIS2_PLACEMENT_3D ( 'NONE', #25652, #2106, #18075 ) ;
#18492 = VERTEX_POINT ( 'NONE', #8752 ) ;
#18493 = DIRECTION ( 'NONE',  ( 0.9980267284282714479, -0.06279051952931540004, 0.000000000000000000 ) ) ;
#18494 = EDGE_CURVE ( 'NONE', #8835, #19766, #14905, .T. ) ;
#18495 = VERTEX_POINT ( 'NONE', #15172 ) ;
#18496 = CARTESIAN_POINT ( 'NONE',  ( -3.999999999999999112, 28.41250000000000497, 11.30940107675849404 ) ) ;
#18497 = VERTEX_POINT ( 'NONE', #5220 ) ;
#18498 = CYLINDRICAL_SURFACE ( 'NONE', #4242, 0.5000000000000004441 ) ;
#18499 = EDGE_CURVE ( 'NONE', #9321, #14559, #11098, .T. ) ;
#18500 = FACE_OUTER_BOUND ( 'NONE', #19739, .T. ) ;
#18501 = ORIENTED_EDGE ( 'NONE', *, *, #24953, .F. ) ;
#18502 = CARTESIAN_POINT ( 'NONE',  ( -29.57785765677917311, 9.610428525061202265, 1.000000000000000000 ) ) ;
#18503 = CARTESIAN_POINT ( 'NONE',  ( -1.878215178124998497, 26.34062499938548285, 12.25316411605951927 ) ) ;
#18504 = DIRECTION ( 'NONE',  ( 1.000000000000000000, 0.000000000000000000, 0.000000000000000000 ) ) ;
#18505 = VECTOR ( 'NONE', #19182, 1000.000000000000000 ) ;
#18506 = DIRECTION ( 'NONE',  ( 1.000000000000000000, 0.000000000000000000, 0.000000000000000000 ) ) ;
#18507 = CARTESIAN_POINT ( 'NONE',  ( 21.65113613650327196, -22.32573188046928436, -2.750000000000000000 ) ) ;
#18508 = DIRECTION ( 'NONE',  ( 0.9510565162951541973, -0.3090169943749456194, 0.000000000000000000 ) ) ;
#18509 = AXIS2_PLACEMENT_3D ( 'NONE', #14012, #17927, #11647 ) ;
#18510 = CARTESIAN_POINT ( 'NONE',  ( -1.878215178124995832, 27.54062499938548214, 5.746835883940462963 ) ) ;
#18511 = CARTESIAN_POINT ( 'NONE',  ( 15.35955758102464408, 20.67195233694332401, 8.999999999999992895 ) ) ;
#18512 = AXIS2_PLACEMENT_3D ( 'NONE', #23411, #13490, #21456 ) ;
#18513 = CARTESIAN_POINT ( 'NONE',  ( 17.55392584295608316, 23.21078009244839180, 8.999999999999992895 ) ) ;
#18514 = CARTESIAN_POINT ( 'NONE',  ( -1.999999999999996669, 25.69374999877097920, 12.46410161513774639 ) ) ;
#18515 = CARTESIAN_POINT ( 'NONE',  ( -1.071796769724488563, 29.31115380933863790, 12.99999999999999289 ) ) ;
#18516 = CARTESIAN_POINT ( 'NONE',  ( -1.878215178125000939, -26.86562499938548498, 12.25316411605952283 ) ) ;
#18517 = CIRCLE ( 'NONE', #22264, 31.10000000000000142 ) ;
#18518 = DIRECTION ( 'NONE',  ( 0.000000000000000000, 0.000000000000000000, 1.000000000000000000 ) ) ;
#18519 = VERTEX_POINT ( 'NONE', #7426 ) ;
#18520 = CARTESIAN_POINT ( 'NONE',  ( 3.756430356250004099, 26.19062499938548783, 6.831223922626973533 ) ) ;
#18521 = CARTESIAN_POINT ( 'NONE',  ( -4.000000000000001776, -29.01249999999999929, 11.30940107675849760 ) ) ;
#18523 = ORIENTED_EDGE ( 'NONE', *, *, #1740, .F. ) ;
#18522 = CARTESIAN_POINT ( 'NONE',  ( 3.756430356250003211, 27.05312499938548854, 8.999999999999992895 ) ) ;
#18524 = EDGE_CURVE ( 'NONE', #1683, #21954, #4947, .T. ) ;
#18525 = ORIENTED_EDGE ( 'NONE', *, *, #18594, .F. ) ;
#18526 = CARTESIAN_POINT ( 'NONE',  ( 3.999999999999995559, -29.18124999877096926, 6.690598923241487306 ) ) ;
#18527 = DIRECTION ( 'NONE',  ( -0.4257792915650642218, 0.9048270524660235736, 0.000000000000000000 ) ) ;
#18528 = ORIENTED_EDGE ( 'NONE', *, *, #5233, .T. ) ;
#18529 = ORIENTED_EDGE ( 'NONE', *, *, #12060, .F. ) ;
#18530 = CARTESIAN_POINT ( 'NONE',  ( 1.878215178124998497, -26.00312499938548783, 12.25316411605951927 ) ) ;
#18531 = EDGE_CURVE ( 'NONE', #18492, #12855, #9277, .T. ) ;
#18532 = CARTESIAN_POINT ( 'NONE',  ( 3.756430356250003211, 28.29062499938548569, 8.999999999999992895 ) ) ;
#18533 = CARTESIAN_POINT ( 'NONE',  ( 0.000000000000000000, -31.10000000000000142, 1.000000000000000000 ) ) ;
#18534 = ADVANCED_FACE ( 'NONE', ( #10974 ), #1549, .F. ) ;
#18535 = CIRCLE ( 'NONE', #6404, 1.500000000000000222 ) ;
#18536 = DIRECTION ( 'NONE',  ( 1.000000000000000000, 0.000000000000000000, 0.000000000000000000 ) ) ;
#18537 = EDGE_CURVE ( 'NONE', #21381, #18175, #11627, .T. ) ;
#18538 = AXIS2_PLACEMENT_3D ( 'NONE', #16086, #18567, #24951 ) ;
#18539 = CYLINDRICAL_SURFACE ( 'NONE', #6, 0.5000000000000004441 ) ;
#18540 = CARTESIAN_POINT ( 'NONE',  ( 1.999999999999995781, -28.30000000000000071, 5.535898384862237620 ) ) ;
#18541 = CARTESIAN_POINT ( 'NONE',  ( 21.21320343559646915, 21.21320343559638744, 4.999999999999992006 ) ) ;
#18542 = DIRECTION ( 'NONE',  ( 0.000000000000000000, 0.000000000000000000, 1.000000000000000000 ) ) ;
#18543 = CARTESIAN_POINT ( 'NONE',  ( 4.000000000000003553, 25.48750000000000071, 6.690598923241489970 ) ) ;
#18544 = CARTESIAN_POINT ( 'NONE',  ( 19.44764619088677549, 19.44764619088670088, 4.662447845253954171 ) ) ;
#18545 = CARTESIAN_POINT ( 'NONE',  ( 18.66319960507342302, 21.49162672981954003, 12.46410161513774639 ) ) ;
#18546 = CARTESIAN_POINT ( 'NONE',  ( -1.499999999999998224, -10.49999999999999289, 30.00000000000000355 ) ) ;
#18547 = DIRECTION ( 'NONE',  ( -0.9048270524660170233, 0.4257792915650782661, 0.000000000000000000 ) ) ;
#18548 = CARTESIAN_POINT ( 'NONE',  ( 3.756430356250004099, 29.34062499938548640, 6.831223922626973533 ) ) ;
#18550 = VERTEX_POINT ( 'NONE', #21170 ) ;
#18549 = DIRECTION ( 'NONE',  ( 0.000000000000000000, 0.000000000000000000, -1.000000000000000000 ) ) ;
#18551 = COLOUR_RGB ( '',0.8941176470588234615, 0.8941176470588234615, 0.8941176470588234615 ) ;
#18552 = DIRECTION ( 'NONE',  ( 0.000000000000000000, 0.000000000000000000, 1.000000000000000000 ) ) ;
#18553 = CARTESIAN_POINT ( 'NONE',  ( 19.03001124868299243, 19.03001124868293559, 4.999999999999991118 ) ) ;
#18554 = VERTEX_POINT ( 'NONE', #1156 ) ;
#18555 = DIRECTION ( 'NONE',  ( 0.000000000000000000, 0.000000000000000000, -1.000000000000000000 ) ) ;
#18556 = CARTESIAN_POINT ( 'NONE',  ( 2.000000000000003997, 26.81874999877096855, 5.535898384862238508 ) ) ;
#18557 = CARTESIAN_POINT ( 'NONE',  ( -1.878215178125004048, -25.66562499938548569, 5.746835883940462963 ) ) ;
#18559 = ORIENTED_EDGE ( 'NONE', *, *, #2262, .T. ) ;
#18558 = DIRECTION ( 'NONE',  ( 0.000000000000000000, 1.000000000000000000, 0.000000000000000000 ) ) ;
#18560 = ORIENTED_EDGE ( 'NONE', *, *, #8340, .T. ) ;
#18561 = CARTESIAN_POINT ( 'NONE',  ( 1.878215178124998497, -26.79062499938548214, 12.25316411605951927 ) ) ;
#18562 = ORIENTED_EDGE ( 'NONE', *, *, #13888, .F. ) ;
#18563 = ORIENTED_EDGE ( 'NONE', *, *, #8779, .F. ) ;
#18564 = LINE ( 'NONE', #16479, #16001 ) ;
#18565 = CARTESIAN_POINT ( 'NONE',  ( -1.878215178124998275, 26.00312499938549493, 12.25316411605951927 ) ) ;
#18566 = EDGE_CURVE ( 'NONE', #6672, #25291, #7046, .T. ) ;
#18567 = DIRECTION ( 'NONE',  ( -0.000000000000000000, -0.000000000000000000, 1.000000000000000000 ) ) ;
#18568 = EDGE_CURVE ( 'NONE', #25106, #7772, #17381, .T. ) ;
#18569 = PRODUCT_DEFINITION_FORMATION_WITH_SPECIFIED_SOURCE ( 'ANY', '', #20064, .NOT_KNOWN. ) ;
#18570 = CARTESIAN_POINT ( 'NONE',  ( -3.756430356249997882, -11.16877607737301226, 1.865624999385482985 ) ) ;
#18571 = CARTESIAN_POINT ( 'NONE',  ( -3.077479918315519036, 38.94082980537690020, 4.370215950314418230 ) ) ;
#18572 = CARTESIAN_POINT ( 'NONE',  ( 1.878215178125000939, 29.67812499938548498, 12.25316411605952283 ) ) ;
#18573 = CARTESIAN_POINT ( 'NONE',  ( 19.82550637751787548, 19.82550637751778666, 12.99999999999999289 ) ) ;
#18574 = CARTESIAN_POINT ( 'NONE',  ( 3.756430356250003211, 25.62812499938548072, 6.831223922626973533 ) ) ;
#18575 =( NAMED_UNIT ( * ) SI_UNIT ( $, .STERADIAN. ) SOLID_ANGLE_UNIT ( ) );
#18576 = CARTESIAN_POINT ( 'NONE',  ( 4.000000000000003553, 25.39374999877096784, 8.999999999999992895 ) ) ;
#18577 = CARTESIAN_POINT ( 'NONE',  ( 3.756430356249997882, -26.86562499938548498, 11.16877607737301226 ) ) ;
#18578 = CARTESIAN_POINT ( 'NONE',  ( -3.999999999999999112, 27.43750000000001066, 6.690598923241487306 ) ) ;
#18579 = DIRECTION ( 'NONE',  ( 0.000000000000000000, 0.000000000000000000, 1.000000000000000000 ) ) ;
#18580 = DIRECTION ( 'NONE',  ( 0.000000000000000000, 0.000000000000000000, -1.000000000000000000 ) ) ;
#18581 = CARTESIAN_POINT ( 'NONE',  ( 4.000096396247766251, -29.73212452601126188, 9.259737768674039415 ) ) ;
#18582 = VERTEX_POINT ( 'NONE', #17126 ) ;
#18583 = CARTESIAN_POINT ( 'NONE',  ( 7.901901826148023498E-15, 27.53124999877097068, 12.99999999999999112 ) ) ;
#18585 = VERTEX_POINT ( 'NONE', #15414 ) ;
#18584 = DIRECTION ( 'NONE',  ( -0.000000000000000000, -0.000000000000000000, 1.000000000000000000 ) ) ;
#18586 = ORIENTED_EDGE ( 'NONE', *, *, #14702, .F. ) ;
#18587 = ORIENTED_EDGE ( 'NONE', *, *, #24712, .T. ) ;
#18588 = ORIENTED_EDGE ( 'NONE', *, *, #14804, .F. ) ;
#18589 = ADVANCED_FACE ( 'NONE', ( #11216 ), #23387, .T. ) ;
#18590 = ORIENTED_EDGE ( 'NONE', *, *, #16159, .F. ) ;
#18591 = ORIENTED_EDGE ( 'NONE', *, *, #8949, .T. ) ;
#18592 = DIRECTION ( 'NONE',  ( -0.000000000000000000, -1.000000000000000000, -0.000000000000000000 ) ) ;
#18593 = CARTESIAN_POINT ( 'NONE',  ( 1.878215178125004048, 28.47812499938548569, 5.746835883940462963 ) ) ;
#18594 = EDGE_CURVE ( 'NONE', #12237, #19902, #7311, .T. ) ;
#18595 = CARTESIAN_POINT ( 'NONE',  ( -3.756430356249996994, -8.999999999999992895, 3.178124999385484983 ) ) ;
#18596 = LINE ( 'NONE', #20553, #9191 ) ;
#18597 = CARTESIAN_POINT ( 'NONE',  ( 21.70382253017380592, 19.04762515221435493, 5.746835883940462963 ) ) ;
#18598 = ADVANCED_FACE ( 'NONE', ( #19458 ), #21299, .F. ) ;
#18599 = CARTESIAN_POINT ( 'NONE',  ( 19.02117241391816904, 21.84959953866428606, 12.46410161513774639 ) ) ;
#18600 = CARTESIAN_POINT ( 'NONE',  ( 3.752267015613588906E-15, -4.381197846482986158, 0.5624999999999986677 ) ) ;
#18601 = AXIS2_PLACEMENT_3D ( 'NONE', #6661, #8755, #8513 ) ;
#18602 = CARTESIAN_POINT ( 'NONE',  ( -1.878215178124998497, -12.25316411605951927, 1.340624999385482630 ) ) ;
#18603 = DIRECTION ( 'NONE',  ( -0.000000000000000000, -0.000000000000000000, 1.000000000000000000 ) ) ;
#18605 = EDGE_CURVE ( 'NONE', #15851, #12275, #13198, .T. ) ;
#18604 = CARTESIAN_POINT ( 'NONE',  ( -1.999999999999998224, -12.46410161513774639, 3.449999999999998401 ) ) ;
#18606 = CARTESIAN_POINT ( 'NONE',  ( 4.000000000000003553, 29.50000000000000355, 8.999999999999992895 ) ) ;
#18607 = CARTESIAN_POINT ( 'NONE',  ( -3.999999999999998224, 29.66874999877097352, 8.999999999999992895 ) ) ;
#18608 = CARTESIAN_POINT ( 'NONE',  ( 3.756430356250003211, -6.831223922626973533, 1.640624999385484895 ) ) ;
#18609 = DIRECTION ( 'NONE',  ( -0.000000000000000000, -0.000000000000000000, 1.000000000000000000 ) ) ;
#18610 = VERTEX_POINT ( 'NONE', #5471 ) ;
#18611 = EDGE_LOOP ( 'NONE', ( #316, #2557, #369, #4764 ) ) ;
#18612 = CARTESIAN_POINT ( 'NONE',  ( -1.878215178124999829, 28.70312499938548711, 12.25316411605951927 ) ) ;
#18613 = VERTEX_POINT ( 'NONE', #13465 ) ;
#18614 = CARTESIAN_POINT ( 'NONE',  ( -7.734255490827218971, -30.12293631110037140, -6.500000000000000000 ) ) ;
#18615 = ORIENTED_EDGE ( 'NONE', *, *, #24680, .F. ) ;
#18616 = DIRECTION ( 'NONE',  ( 1.000000000000000000, 0.000000000000000000, 0.000000000000000000 ) ) ;
#18617 = VERTEX_POINT ( 'NONE', #21432 ) ;
#18618 = DIRECTION ( 'NONE',  ( -0.000000000000000000, -0.000000000000000000, 1.000000000000000000 ) ) ;
#18619 = DIRECTION ( 'NONE',  ( 1.000000000000000000, 0.000000000000000000, 0.000000000000000000 ) ) ;
#18620 = ORIENTED_EDGE ( 'NONE', *, *, #5330, .T. ) ;
#18621 = CARTESIAN_POINT ( 'NONE',  ( -0.07783014623660702846, 38.99999999999950262, 14.50000000000044587 ) ) ;
#18622 =( BOUNDED_CURVE ( )  B_SPLINE_CURVE ( 2, ( #17134, #23394, #11610, #11224, #15294, #7571, #23262 ),
 .UNSPECIFIED., .F., .F. ) 
 B_SPLINE_CURVE_WITH_KNOTS ( ( 3, 2, 2, 3 ),
 ( 0.9500000000000003997, 0.9666666666666670071, 0.9833333333333333925, 1.000000000000000000 ),
 .UNSPECIFIED. ) 
 CURVE ( )  GEOMETRIC_REPRESENTATION_ITEM ( )  RATIONAL_B_SPLINE_CURVE ( ( 0.9999999999999964473, 0.8660254037844422603, 1.000000000000000000, 0.8660254037844387076, 1.000000000000000000, 0.8660254037844387076, 1.000000000000000000 ) ) 
 REPRESENTATION_ITEM ( '' )  );
#18623 = CARTESIAN_POINT ( 'NONE',  ( 3.752267015613588906E-15, 25.11250000000000071, 4.381197846482986158 ) ) ;
#18624 = CARTESIAN_POINT ( 'NONE',  ( 3.469446951953614189E-15, 30.00000000000000355, 8.999999999999992895 ) ) ;
#18625 = CARTESIAN_POINT ( 'NONE',  ( 4.000000000000003553, 26.80000000000000071, 8.999999999999992895 ) ) ;
#18626 = CARTESIAN_POINT ( 'NONE',  ( 15.98945208958084407, 21.64630633907315982, 11.30940107675849404 ) ) ;
#18627 = FACE_OUTER_BOUND ( 'NONE', #9798, .T. ) ;
#18628 =( BOUNDED_CURVE ( )  B_SPLINE_CURVE ( 2, ( #7009, #22845, #744, #22723, #8713, #22588, #24671, #20879, #18925 ),
 .UNSPECIFIED., .F., .F. ) 
 B_SPLINE_CURVE_WITH_KNOTS ( ( 3, 2, 2, 2, 3 ),
 ( 0.6250000000000000000, 0.6333333333333333037, 0.6500000000000000222, 0.6666666666666666297, 0.6750000000000000444 ),
 .UNSPECIFIED. ) 
 CURVE ( )  GEOMETRIC_REPRESENTATION_ITEM ( )  RATIONAL_B_SPLINE_CURVE ( ( 0.9330127018922194093, 0.9330127018922194093, 1.000000000000000000, 0.8660254037844387076, 1.000000000000000000, 0.8660254037844387076, 1.000000000000000000, 0.9330127018922189652, 0.9330127018922194093 ) ) 
 REPRESENTATION_ITEM ( '' )  );
#18629 = EDGE_CURVE ( 'NONE', #10460, #5837, #3513, .T. ) ;
#18630 = CARTESIAN_POINT ( 'NONE',  ( 3.756430356250003655, 27.84062499938548640, 8.999999999999992895 ) ) ;
#18631 = EDGE_CURVE ( 'NONE', #5488, #20241, #24145, .T. ) ;
#18632 = CARTESIAN_POINT ( 'NONE',  ( 3.469446951953614189E-15, 25.00000000000000000, 8.999999999999992895 ) ) ;
#18633 = CARTESIAN_POINT ( 'NONE',  ( 0.4999838450259763700, -31.09598070739550124, -2.750000000000000000 ) ) ;
#18634 = DIRECTION ( 'NONE',  ( 1.000000000000000000, 0.000000000000000000, 0.000000000000000000 ) ) ;
#18635 = ADVANCED_FACE ( 'NONE', ( #5097 ), #18956, .F. ) ;
#18636 = FACE_OUTER_BOUND ( 'NONE', #14920, .T. ) ;
#18637 = CARTESIAN_POINT ( 'NONE',  ( 1.878215178124995832, -27.54062499938548214, 5.746835883940462963 ) ) ;
#18638 = EDGE_CURVE ( 'NONE', #10717, #5108, #9558, .T. ) ;
#18639 = VERTEX_POINT ( 'NONE', #3762 ) ;
#18640 = CARTESIAN_POINT ( 'NONE',  ( 2.672651547586948120E-15, 26.49062499938548143, 13.33755215474602984 ) ) ;
#18641 = CARTESIAN_POINT ( 'NONE',  ( 22.40202671059728345, 16.74517246110483271, 6.690598923241489970 ) ) ;
#18643 = VERTEX_POINT ( 'NONE', #21677 ) ;
#18642 = CARTESIAN_POINT ( 'NONE',  ( 4.006172263299091013E-15, 28.96562499938549351, 4.662447845253954171 ) ) ;
#18644 = ORIENTED_EDGE ( 'NONE', *, *, #2367, .T. ) ;
#18645 = CARTESIAN_POINT ( 'NONE',  ( 3.469446951953614189E-15, 30.00000000000000355, 4.999999999999992006 ) ) ;
#18646 = CARTESIAN_POINT ( 'NONE',  ( 1.500000000000000222, 0.000000000000000000, 18.19999999999999929 ) ) ;
#18647 = EDGE_LOOP ( 'NONE', ( #12174, #2279, #18178, #3587 ) ) ;
#18648 = CARTESIAN_POINT ( 'NONE',  ( -3.735045420075836212E-15, -26.26562499938548356, 4.662447845253954171 ) ) ;
#18649 = CARTESIAN_POINT ( 'NONE',  ( 26.00000000000000711, 3.184081677783118980E-15, 19.50000000000000000 ) ) ;
#18650 = DIRECTION ( 'NONE',  ( 0.000000000000000000, 1.000000000000000000, 0.000000000000000000 ) ) ;
#18651 = CARTESIAN_POINT ( 'NONE',  ( -1.878215178124998275, 26.79062499938548569, 12.25316411605951927 ) ) ;
#18652 = CARTESIAN_POINT ( 'NONE',  ( 23.33010436090463102, 17.67325011141217317, 8.999999999999992895 ) ) ;
#18653 = CARTESIAN_POINT ( 'NONE',  ( 5.840899737312971851, 31.50000000000000000, 7.627451181685208859 ) ) ;
#18654 = ADVANCED_FACE ( 'NONE', ( #23643 ), #5854, .T. ) ;
#18655 = LINE ( 'NONE', #10542, #12170 ) ;
#18656 = CARTESIAN_POINT ( 'NONE',  ( 3.756430356250002323, 25.55312499938548498, 11.16877607737301403 ) ) ;
#18657 = DIRECTION ( 'NONE',  ( 1.000000000000000000, 0.000000000000000000, 0.000000000000000000 ) ) ;
#18658 = CARTESIAN_POINT ( 'NONE',  ( 18.57032807491351178, 21.22652545287281356, 12.25316411605951927 ) ) ;
#18659 = CARTESIAN_POINT ( 'NONE',  ( 16.63462326141533865, 19.29082063937464397, 5.746835883940462963 ) ) ;
#18660 = CARTESIAN_POINT ( 'NONE',  ( 20.50609665440990526, 14.84924240491746339, 8.999999999999992895 ) ) ;
#18661 = CARTESIAN_POINT ( 'NONE',  ( 0.000000000000000000, 0.000000000000000000, 1.000000000000000000 ) ) ;
#18662 = CARTESIAN_POINT ( 'NONE',  ( 2.672651547586948120E-15, 29.19062499938548783, 13.33755215474602984 ) ) ;
#18664 = ORIENTED_EDGE ( 'NONE', *, *, #14332, .T. ) ;
#18663 = DIRECTION ( 'NONE',  ( 0.000000000000000000, 0.000000000000000000, 1.000000000000000000 ) ) ;
#18665 = DIRECTION ( 'NONE',  ( 0.000000000000000000, 0.000000000000000000, 1.000000000000000000 ) ) ;
#18666 = CARTESIAN_POINT ( 'NONE',  ( 20.31164228958361306, 17.48321516483735394, 12.46410161513774817 ) ) ;
#18667 = ORIENTED_EDGE ( 'NONE', *, *, #9765, .F. ) ;
#18668 = CARTESIAN_POINT ( 'NONE',  ( 11.91206721063030649, -28.72825533807137433, -6.500000000000000000 ) ) ;
#18669 = CARTESIAN_POINT ( 'NONE',  ( 3.752267015613588906E-15, 26.85624999877096641, 4.381197846482986158 ) ) ;
#18670 = CARTESIAN_POINT ( 'NONE',  ( 1.878215178124998497, -27.69062499938548427, 12.25316411605951927 ) ) ;
#18672 = ORIENTED_EDGE ( 'NONE', *, *, #19464, .T. ) ;
#18671 = DIRECTION ( 'NONE',  ( 1.000000000000000000, 0.000000000000000000, 0.000000000000000000 ) ) ;
#18673 = CARTESIAN_POINT ( 'NONE',  ( 4.000000000000000888, 29.85624999877096997, 11.30940107675849760 ) ) ;
#18674 = EDGE_CURVE ( 'NONE', #20151, #18519, #358, .T. ) ;
#18675 = ORIENTED_EDGE ( 'NONE', *, *, #22775, .F. ) ;
#18676 = CARTESIAN_POINT ( 'NONE',  ( 1.878215178124995832, -25.29062499938548569, 5.746835883940462963 ) ) ;
#18677 = VERTEX_POINT ( 'NONE', #2063 ) ;
#18678 = ORIENTED_EDGE ( 'NONE', *, *, #10146, .F. ) ;
#18679 = FILL_AREA_STYLE ('',( #764 ) ) ;
#18680 = CARTESIAN_POINT ( 'NONE',  ( 21.21320343559646915, 21.21320343559638744, 8.999999999999992895 ) ) ;
#18681 = CARTESIAN_POINT ( 'NONE',  ( 4.000000000000001776, 27.66249999999999787, 11.30940107675849760 ) ) ;
#18682 = CARTESIAN_POINT ( 'NONE',  ( -3.756430356249996994, -8.999999999999992895, 2.728124999385482585 ) ) ;
#18683 = CYLINDRICAL_SURFACE ( 'NONE', #12614, 31.10000000000000142 ) ;
#18684 = CARTESIAN_POINT ( 'NONE',  ( -1.878215178124995832, 28.89062499938548356, 5.746835883940462963 ) ) ;
#18685 = CARTESIAN_POINT ( 'NONE',  ( -30.35476721088030061, -3.897863563849544466, 1.000000000000000000 ) ) ;
#18686 = CARTESIAN_POINT ( 'NONE',  ( 4.000000000000003553, -8.999999999999992895, 0.8437499987709664584 ) ) ;
#18687 = CARTESIAN_POINT ( 'NONE',  ( -3.756430356249997438, 29.00312499938548072, 11.16877607737301048 ) ) ;
#18688 = FACE_OUTER_BOUND ( 'NONE', #10283, .T. ) ;
#18689 = DIRECTION ( 'NONE',  ( 0.000000000000000000, -0.000000000000000000, 1.000000000000000000 ) ) ;
#18690 = CARTESIAN_POINT ( 'NONE',  ( 0.000000000000000000, 0.000000000000000000, -6.500000000000000000 ) ) ;
#18691 = CARTESIAN_POINT ( 'NONE',  ( -3.735045420075836212E-15, -25.81562499938548783, 4.662447845253954171 ) ) ;
#18692 =( BOUNDED_CURVE ( )  B_SPLINE_CURVE ( 2, ( #8925, #16905, #24869, #21329, #15579 ),
 .UNSPECIFIED., .F., .F. ) 
 B_SPLINE_CURVE_WITH_KNOTS ( ( 3, 2, 3 ),
 ( 0.000000000000000000, 0.01666666666666666644, 0.02500000000000000486 ),
 .UNSPECIFIED. ) 
 CURVE ( )  GEOMETRIC_REPRESENTATION_ITEM ( )  RATIONAL_B_SPLINE_CURVE ( ( 1.000000000000000000, 0.8660254037844387076, 1.000000000000000000, 0.9330127018922194093, 0.9330127018922194093 ) ) 
 REPRESENTATION_ITEM ( '' )  );
#18693 = DIRECTION ( 'NONE',  ( 0.000000000000000000, 0.000000000000000000, 1.000000000000000000 ) ) ;
#18694 = DIRECTION ( 'NONE',  ( 0.000000000000000000, 0.000000000000000000, 1.000000000000000000 ) ) ;
#18695 = DIRECTION ( 'NONE',  ( 0.000000000000000000, 0.000000000000000000, 1.000000000000000000 ) ) ;
#18696 = CARTESIAN_POINT ( 'NONE',  ( -1.071796769724481901, 28.01740381056766438, 12.99999999999999645 ) ) ;
#18697 = EDGE_CURVE ( 'NONE', #3646, #1770, #14115, .T. ) ;
#18698 = VERTEX_POINT ( 'NONE', #115 ) ;
#18700 = ORIENTED_EDGE ( 'NONE', *, *, #15787, .T. ) ;
#18699 = CARTESIAN_POINT ( 'NONE',  ( -18.68225429291750928, -24.86329371854754200, -2.750000000000000000 ) ) ;
#18701 = VERTEX_POINT ( 'NONE', #21551 ) ;
#18702 = AXIS2_PLACEMENT_3D ( 'NONE', #1098, #6982, #14963 ) ;
#18703 = EDGE_LOOP ( 'NONE', ( #16536, #19472, #8797 ) ) ;
#18704 = EDGE_LOOP ( 'NONE', ( #16067, #10120 ) ) ;
#18705 = VERTEX_POINT ( 'NONE', #7563 ) ;
#18706 = DIRECTION ( 'NONE',  ( 0.000000000000000000, 0.000000000000000000, -1.000000000000000000 ) ) ;
#18707 = ORIENTED_EDGE ( 'NONE', *, *, #19537, .T. ) ;
#18708 = CARTESIAN_POINT ( 'NONE',  ( 5.840899737312971851, 38.49999999999999289, 7.627451181685208859 ) ) ;
#18709 = CARTESIAN_POINT ( 'NONE',  ( -3.756430356249997438, 27.76562499938549067, 11.16877607737301048 ) ) ;
#18710 = CARTESIAN_POINT ( 'NONE',  ( 2.672651547586948120E-15, -13.33755215474602984, 1.378124999385482274 ) ) ;
#18711 = CARTESIAN_POINT ( 'NONE',  ( 19.34820930021694352, 19.34820930021687246, 4.999999999999992006 ) ) ;
#18712 = CARTESIAN_POINT ( 'NONE',  ( 18.17030703624117294, 23.48270179215984754, 11.16877607737301226 ) ) ;
#18713 = CARTESIAN_POINT ( 'NONE',  ( -1.878215178124995832, 26.30312499938548498, 5.746835883940462963 ) ) ;
#18714 = CARTESIAN_POINT ( 'NONE',  ( 14.54246377227340048, -27.49048467073863833, -6.500000000000000000 ) ) ;
#18715 = CIRCLE ( 'NONE', #11595, 31.10000000000000142 ) ;
#18716 = CARTESIAN_POINT ( 'NONE',  ( 3.756430356250004099, -6.831223922626973533, 3.778124999385480631 ) ) ;
#18717 = EDGE_CURVE ( 'NONE', #10619, #18643, #17907, .T. ) ;
#18718 = LINE ( 'NONE', #5132, #5021 ) ;
#18719 = CARTESIAN_POINT ( 'NONE',  ( 1.626862140677534194E-14, 27.98124999877096997, 12.99999999999999289 ) ) ;
#18720 = DIRECTION ( 'NONE',  ( 1.000000000000000000, 0.000000000000000000, 0.000000000000000000 ) ) ;
#18721 = CARTESIAN_POINT ( 'NONE',  ( -1.999999999999996669, 29.74374999877097636, 12.46410161513774639 ) ) ;
#18722 = CARTESIAN_POINT ( 'NONE',  ( 3.756430356250003211, -6.831223922626973533, 2.990624999385483651 ) ) ;
#18723 = FACE_OUTER_BOUND ( 'NONE', #19385, .T. ) ;
#18724 = EDGE_CURVE ( 'NONE', #24543, #10117, #11603, .T. ) ;
#18725 = VECTOR ( 'NONE', #7601, 1000.000000000000000 ) ;
#18726 = DIRECTION ( 'NONE',  ( -0.7071067811865487940, -0.7071067811865463515, 0.000000000000000000 ) ) ;
#18727 = VERTEX_POINT ( 'NONE', #15675 ) ;
#18728 = ORIENTED_EDGE ( 'NONE', *, *, #2288, .T. ) ;
#18729 = CARTESIAN_POINT ( 'NONE',  ( 3.756430356250001434, 27.50312499938548783, 8.999999999999992895 ) ) ;
#18730 = EDGE_CURVE ( 'NONE', #7828, #21834, #15795, .T. ) ;
#18731 = ORIENTED_EDGE ( 'NONE', *, *, #579, .F. ) ;
#18732 = DIRECTION ( 'NONE',  ( -0.000000000000000000, -1.000000000000000000, -0.000000000000000000 ) ) ;
#18733 = VERTEX_POINT ( 'NONE', #4145 ) ;
#18734 = DIRECTION ( 'NONE',  ( 0.000000000000000000, 0.000000000000000000, 1.000000000000000000 ) ) ;
#18735 = EDGE_CURVE ( 'NONE', #246, #1590, #24028, .T. ) ;
#18736 = ORIENTED_EDGE ( 'NONE', *, *, #1321, .F. ) ;
#18737 = DIRECTION ( 'NONE',  ( -0.000000000000000000, -1.000000000000000000, -0.000000000000000000 ) ) ;
#18738 = AXIS2_PLACEMENT_3D ( 'NONE', #8477, #12129, #6501 ) ;
#18739 = ORIENTED_EDGE ( 'NONE', *, *, #17500, .F. ) ;
#18740 = VECTOR ( 'NONE', #21907, 1000.000000000000000 ) ;
#18741 = EDGE_CURVE ( 'NONE', #21732, #14041, #8085, .T. ) ;
#18742 = DIRECTION ( 'NONE',  ( -1.000000000000000000, 0.000000000000000000, 0.000000000000000000 ) ) ;
#18743 = CARTESIAN_POINT ( 'NONE',  ( 4.000000000000003553, 25.03749999999999787, 6.690598923241489970 ) ) ;
#18744 = CARTESIAN_POINT ( 'NONE',  ( 18.68225429291721795, 24.86329371854775161, 1.000000000000000000 ) ) ;
#18745 = VECTOR ( 'NONE', #893, 1000.000000000000000 ) ;
#18746 = CIRCLE ( 'NONE', #9125, 0.5000000000000001110 ) ;
#18747 = LINE ( 'NONE', #16805, #11749 ) ;
#18748 = CARTESIAN_POINT ( 'NONE',  ( 16.95054783869437642, 22.26294259461305103, 8.999999999999992895 ) ) ;
#18749 = CARTESIAN_POINT ( 'NONE',  ( 3.756430356250002323, 29.15312499938548640, 11.16877607737301226 ) ) ;
#18750 = CARTESIAN_POINT ( 'NONE',  ( 18.25440349763447756, 18.25440349763440651, 4.662447845253954171 ) ) ;
#18751 = DIRECTION ( 'NONE',  ( -0.000000000000000000, -0.000000000000000000, 1.000000000000000000 ) ) ;
#18752 = AXIS2_PLACEMENT_3D ( 'NONE', #22005, #19652, #7757 ) ;
#18753 = ORIENTED_EDGE ( 'NONE', *, *, #24712, .F. ) ;
#18754 = CARTESIAN_POINT ( 'NONE',  ( -4.000000000000003553, -25.03750000000000142, 6.690598923241489970 ) ) ;
#18755 = CARTESIAN_POINT ( 'NONE',  ( -1.999999999999994893, 26.44374999877097210, 5.535898384862237620 ) ) ;
#18756 = CARTESIAN_POINT ( 'NONE',  ( 3.369928719974892281E-15, 25.50624999877096855, 4.999999999999992006 ) ) ;
#18758 = CARTESIAN_POINT ( 'NONE',  ( -3.756430356250003211, -28.32812499938548356, 6.831223922626973533 ) ) ;
#18757 = AXIS2_PLACEMENT_3D ( 'NONE', #19261, #17435, #21741 ) ;
#18759 = DIRECTION ( 'NONE',  ( 1.000000000000000000, 0.000000000000000000, 0.000000000000000000 ) ) ;
#18760 = CIRCLE ( 'NONE', #15431, 0.4999999999999997224 ) ;
#18761 = CARTESIAN_POINT ( 'NONE',  ( 1.878215178125004048, 26.22812499938548569, 5.746835883940462963 ) ) ;
#18762 = CARTESIAN_POINT ( 'NONE',  ( -3.469446951953614189E-15, -30.00000000000000355, 8.999999999999992895 ) ) ;
#18764 = VERTEX_POINT ( 'NONE', #13701 ) ;
#18763 = CARTESIAN_POINT ( 'NONE',  ( 0.000000000000000000, 0.000000000000000000, 1.000000000000000000 ) ) ;
#18765 = ORIENTED_EDGE ( 'NONE', *, *, #18449, .T. ) ;
#18766 =( BOUNDED_CURVE ( )  B_SPLINE_CURVE ( 2, ( #3011, #784, #664, #24851, #14653, #4444, #8375, #18450, #10708 ),
 .UNSPECIFIED., .F., .F. ) 
 B_SPLINE_CURVE_WITH_KNOTS ( ( 3, 2, 2, 2, 3 ),
 ( 0.02500000000000000139, 0.03333333333333333287, 0.05000000000000000278, 0.06666666666666666574, 0.07500000000000001110 ),
 .UNSPECIFIED. ) 
 CURVE ( )  GEOMETRIC_REPRESENTATION_ITEM ( )  RATIONAL_B_SPLINE_CURVE ( ( 0.9330127018922194093, 0.9330127018922194093, 1.000000000000000000, 0.8660254037844387076, 1.000000000000000000, 0.8660254037844387076, 1.000000000000000000, 0.9330127018922191873, 0.9330127018922192983 ) ) 
 REPRESENTATION_ITEM ( '' )  );
#18767 = CARTESIAN_POINT ( 'NONE',  ( 1.999999999999995781, -29.14374999877096784, 5.535898384862237620 ) ) ;
#18768 = FACE_OUTER_BOUND ( 'NONE', #8870, .T. ) ;
#18769 = ORIENTED_EDGE ( 'NONE', *, *, #19950, .F. ) ;
#18770 = ADVANCED_FACE ( 'NONE', ( #10031 ), #16947, .F. ) ;
#18771 = CARTESIAN_POINT ( 'NONE',  ( -1.878215178125004048, -27.12812499938548783, 5.746835883940462963 ) ) ;
#18772 = CARTESIAN_POINT ( 'NONE',  ( 6.009258394948636914E-15, 29.30312499938549564, 4.662447845253954171 ) ) ;
#18773 =( BOUNDED_CURVE ( )  B_SPLINE_CURVE ( 2, ( #23745, #5833, #13821, #3880, #19822, #12457, #1530, #9501, #1923 ),
 .UNSPECIFIED., .F., .F. ) 
 B_SPLINE_CURVE_WITH_KNOTS ( ( 3, 2, 2, 2, 3 ),
 ( 0.9250000000000000444, 0.9333333333333333481, 0.9499999999999999556, 0.9666666666666666741, 0.9749999999999999778 ),
 .UNSPECIFIED. ) 
 CURVE ( )  GEOMETRIC_REPRESENTATION_ITEM ( )  RATIONAL_B_SPLINE_CURVE ( ( 0.9330127018922194093, 0.9330127018922198534, 1.000000000000000000, 0.8660254037844387076, 1.000000000000000000, 0.8660254037844387076, 1.000000000000000000, 0.9330127018922194093, 0.9330127018922194093 ) ) 
 REPRESENTATION_ITEM ( '' )  );
#18774 = CARTESIAN_POINT ( 'NONE',  ( -3.756430356249996549, 25.40312499938548640, 11.16877607737301048 ) ) ;
#18775 = AXIS2_PLACEMENT_3D ( 'NONE', #740, #8709, #2963 ) ;
#18776 = EDGE_CURVE ( 'NONE', #11111, #22395, #4371, .T. ) ;
#18777 = CARTESIAN_POINT ( 'NONE',  ( 2.000000000000000000, 26.27500000000000568, 12.46410161513774817 ) ) ;
#18778 = CARTESIAN_POINT ( 'NONE',  ( -4.000000000000000888, 25.71250000000000568, 11.30940107675849404 ) ) ;
#18779 = AXIS2_PLACEMENT_3D ( 'NONE', #25852, #19952, #1672 ) ;
#18780 = CARTESIAN_POINT ( 'NONE',  ( -1.878215178124998497, -12.25316411605951927, 4.040624999385483918 ) ) ;
#18781 = VECTOR ( 'NONE', #11293, 1000.000000000000000 ) ;
#18782 = FACE_OUTER_BOUND ( 'NONE', #2491, .T. ) ;
#18783 = CARTESIAN_POINT ( 'NONE',  ( 0.000000000000000000, 0.000000000000000000, 0.000000000000000000 ) ) ;
#18784 = DIRECTION ( 'NONE',  ( -0.000000000000000000, -1.000000000000000000, -0.000000000000000000 ) ) ;
#18785 = CARTESIAN_POINT ( 'NONE',  ( 3.469446951953614189E-15, 34.00000000000000000, 3.499999999999992895 ) ) ;
#18786 = CARTESIAN_POINT ( 'NONE',  ( 2.672651547586948120E-15, 25.47812499938548569, 13.33755215474603162 ) ) ;
#18787 = VECTOR ( 'NONE', #6416, 1000.000000000000000 ) ;
#18788 = CARTESIAN_POINT ( 'NONE',  ( 0.000000000000000000, 0.000000000000000000, 1.000000000000000000 ) ) ;
#18789 = CARTESIAN_POINT ( 'NONE',  ( 23.58876780933789519, 18.27637305341907492, 11.16877607737301226 ) ) ;
#18790 = CARTESIAN_POINT ( 'NONE',  ( 17.05888733012726632, 19.71508470808657520, 12.25316411605951927 ) ) ;
#18791 = FACE_OUTER_BOUND ( 'NONE', #3746, .T. ) ;
#18792 = CARTESIAN_POINT ( 'NONE',  ( -13.24173596767339767, 28.14012133169338270, -6.500000000000000000 ) ) ;
#18793 = CARTESIAN_POINT ( 'NONE',  ( -1.878215178124998497, 27.69062499938548427, 12.25316411605951927 ) ) ;
#18794 = CIRCLE ( 'NONE', #15054, 4.000000000000000000 ) ;
#18795 = DIRECTION ( 'NONE',  ( 0.000000000000000000, 1.000000000000000000, 0.000000000000000000 ) ) ;
#18796 = LINE ( 'NONE', #20757, #4975 ) ;
#18797 = CARTESIAN_POINT ( 'NONE',  ( 2.000000000000000888, -12.46410161513774817, 3.075000000000001510 ) ) ;
#18798 = ORIENTED_EDGE ( 'NONE', *, *, #9343, .T. ) ;
#18799 = CARTESIAN_POINT ( 'NONE',  ( -5.840899737312954976, 31.50000000000000000, 10.37254881831481690 ) ) ;
#18800 = CARTESIAN_POINT ( 'NONE',  ( 2.000000000000003997, 29.06874999877096855, 5.535898384862238508 ) ) ;
#18801 = CARTESIAN_POINT ( 'NONE',  ( 1.878215178124995832, -28.89062499938548356, 5.746835883940462963 ) ) ;
#18803 = ORIENTED_EDGE ( 'NONE', *, *, #2666, .T. ) ;
#18802 = CARTESIAN_POINT ( 'NONE',  ( -3.999999999999996447, 25.61874999877096926, 8.999999999999992895 ) ) ;
#18804 = CARTESIAN_POINT ( 'NONE',  ( 0.000000000000000000, 0.000000000000000000, -6.500000000000000000 ) ) ;
#18805 = MECHANICAL_DESIGN_GEOMETRIC_PRESENTATION_REPRESENTATION (  '', ( #17533 ), #22963 ) ;
#18806 = ORIENTED_EDGE ( 'NONE', *, *, #8590, .F. ) ;
#18807 = ADVANCED_FACE ( 'NONE', ( #22416 ), #24508, .F. ) ;
#18808 = CARTESIAN_POINT ( 'NONE',  ( 3.756430356249996994, -26.71562499938548285, 8.999999999999992895 ) ) ;
#18809 = ORIENTED_EDGE ( 'NONE', *, *, #19307, .F. ) ;
#18810 = VERTEX_POINT ( 'NONE', #22164 ) ;
#18811 = CARTESIAN_POINT ( 'NONE',  ( 0.000000000000000000, 0.000000000000000000, -6.500000000000000000 ) ) ;
#18812 = CARTESIAN_POINT ( 'NONE',  ( -1.878215178124998275, 28.10312499938548925, 5.746835883940462963 ) ) ;
#18813 = EDGE_CURVE ( 'NONE', #4477, #16624, #16154, .T. ) ;
#18814 = AXIS2_PLACEMENT_3D ( 'NONE', #13784, #3583, #1622 ) ;
#18815 = DIRECTION ( 'NONE',  ( 1.000000000000000000, 0.000000000000000000, 0.000000000000000000 ) ) ;
#18816 = CIRCLE ( 'NONE', #4625, 31.10000000000000142 ) ;
#18817 = AXIS2_PLACEMENT_3D ( 'NONE', #21407, #17475, #19815 ) ;
#18818 = CARTESIAN_POINT ( 'NONE',  ( 2.672651547586948120E-15, -13.33755215474602984, 1.490624999385481209 ) ) ;
#18819 = CARTESIAN_POINT ( 'NONE',  ( -3.290218409505503150, 38.99776139129450314, 4.589573109331187339 ) ) ;
#18820 = CARTESIAN_POINT ( 'NONE',  ( -1.878215178124998497, 28.14062499938548356, 12.25316411605951927 ) ) ;
#18821 = AXIS2_PLACEMENT_3D ( 'NONE', #21746, #13766, #3829 ) ;
#18822 = CARTESIAN_POINT ( 'NONE',  ( 21.36466611845514052, 19.84891659060301805, 4.999999999999988454 ) ) ;
#18823 = CARTESIAN_POINT ( 'NONE',  ( -7.734255490826573265, 30.12293631110053838, 1.000000000000000000 ) ) ;
#18824 = UNCERTAINTY_MEASURE_WITH_UNIT (LENGTH_MEASURE( 1.000000000000000082E-05 ), #9270, 'distance_accuracy_value', 'NONE');
#18825 = CARTESIAN_POINT ( 'NONE',  ( 2.672651547586948120E-15, 29.52812499938548285, 13.33755215474603162 ) ) ;
#18826 = CARTESIAN_POINT ( 'NONE',  ( 12.78762572734037484, -28.34936733434209444, -2.750000000000000000 ) ) ;
#18827 = CARTESIAN_POINT ( 'NONE',  ( 22.01336592481439780, 20.38367064973063236, 12.84165680230635864 ) ) ;
#18828 = FACE_OUTER_BOUND ( 'NONE', #14551, .T. ) ;
#18829 = CARTESIAN_POINT ( 'NONE',  ( 15.26024822061316577, 20.91710247010547619, 6.690598923241487306 ) ) ;
#18830 = CARTESIAN_POINT ( 'NONE',  ( -3.756430356250002323, -27.91562499938548569, 11.16877607737301226 ) ) ;
#18831 = CARTESIAN_POINT ( 'NONE',  ( 3.756430356250002323, 26.11562499938548498, 11.16877607737301226 ) ) ;
#18832 = DIRECTION ( 'NONE',  ( -0.000000000000000000, -0.000000000000000000, 1.000000000000000000 ) ) ;
#18833 = AXIS2_PLACEMENT_3D ( 'NONE', #9639, #14077, #19943 ) ;
#18834 = CARTESIAN_POINT ( 'NONE',  ( -29.62293631110050995, -7.734255490826679846, 1.000000000000000000 ) ) ;
#18835 = CARTESIAN_POINT ( 'NONE',  ( 23.02516456238698339, 17.36831031289453264, 11.30940107675849760 ) ) ;
#18836 = EDGE_LOOP ( 'NONE', ( #12236, #17831, #4621, #10991 ) ) ;
#18837 = CARTESIAN_POINT ( 'NONE',  ( 4.000000000000003553, 27.64374999877097139, 8.999999999999992895 ) ) ;
#18839 = ORIENTED_EDGE ( 'NONE', *, *, #18073, .F. ) ;
#18838 = CARTESIAN_POINT ( 'NONE',  ( 25.45105997952912702, -17.87326343783951899, 1.000000000000000000 ) ) ;
#18840 = CIRCLE ( 'NONE', #3394, 31.10000000000000142 ) ;
#18841 = AXIS2_PLACEMENT_3D ( 'NONE', #16390, #10608, #22625 ) ;
#18842 = ORIENTED_EDGE ( 'NONE', *, *, #22255, .T. ) ;
#18843 = ORIENTED_EDGE ( 'NONE', *, *, #8568, .F. ) ;
#18844 = ORIENTED_EDGE ( 'NONE', *, *, #314, .T. ) ;
#18845 = ORIENTED_EDGE ( 'NONE', *, *, #9124, .F. ) ;
#18846 = AXIS2_PLACEMENT_3D ( 'NONE', #5178, #13154, #3197 ) ;
#18847 = EDGE_CURVE ( 'NONE', #22527, #12823, #16108, .T. ) ;
#18848 = LINE ( 'NONE', #8527, #4266 ) ;
#18849 = ORIENTED_EDGE ( 'NONE', *, *, #15926, .F. ) ;
#18850 = CARTESIAN_POINT ( 'NONE',  ( 0.000000000000000000, 0.000000000000000000, 1.000000000000000000 ) ) ;
#18851 = CARTESIAN_POINT ( 'NONE',  ( 1.878215178125004048, 28.92812499938548854, 5.746835883940462963 ) ) ;
#18852 = EDGE_CURVE ( 'NONE', #12855, #25184, #3690, .T. ) ;
#18853 = AXIS2_PLACEMENT_3D ( 'NONE', #20310, #14708, #12742 ) ;
#18854 = CARTESIAN_POINT ( 'NONE',  ( -1.878215178124995832, -5.746835883940462963, 4.453124999385483562 ) ) ;
#18855 = CARTESIAN_POINT ( 'NONE',  ( -3.999999999999996003, -6.690598923241487306, 0.5812499987709676130 ) ) ;
#18856 = PRODUCT_DEFINITION_SHAPE ( 'NONE', 'NONE',  #25877 ) ;
#18857 = CARTESIAN_POINT ( 'NONE',  ( 17.50739442887878639, 22.81978918479745744, 8.999999999999992895 ) ) ;
#18858 = VECTOR ( 'NONE', #9528, 1000.000000000000000 ) ;
#18859 = CARTESIAN_POINT ( 'NONE',  ( 3.756430356250004099, 26.64062499938549067, 6.831223922626973533 ) ) ;
#18860 = VECTOR ( 'NONE', #8271, 999.9999999999998863 ) ;
#18861 = EDGE_CURVE ( 'NONE', #20629, #22953, #20063, .T. ) ;
#18862 = CARTESIAN_POINT ( 'NONE',  ( -5.532151103383255553, 34.50000000000000000, 6.677220593914389823 ) ) ;
#18863 = CARTESIAN_POINT ( 'NONE',  ( -1.878215178124998497, -12.25316411605951927, 3.140624999385482230 ) ) ;
#18864 = CYLINDRICAL_SURFACE ( 'NONE', #18383, 4.000000000000000000 ) ;
#18865 = CARTESIAN_POINT ( 'NONE',  ( -3.999999999999997335, -11.30940107675849404, 4.312500000000000000 ) ) ;
#18866 = CARTESIAN_POINT ( 'NONE',  ( -5.840899737312982509, 38.49999999999999289, 7.627451181685283466 ) ) ;
#18867 = CARTESIAN_POINT ( 'NONE',  ( 3.469446951953614189E-15, 30.00000000000000355, 4.999999999999992006 ) ) ;
#18868 = CARTESIAN_POINT ( 'NONE',  ( 2.672651547586948120E-15, -13.33755215474603162, 2.840624999385484628 ) ) ;
#18869 = CARTESIAN_POINT ( 'NONE',  ( 3.718542035834364277E-15, 25.11250000000000782, 4.999999999999992006 ) ) ;
#18870 = CARTESIAN_POINT ( 'NONE',  ( 23.69483382651587888, 18.38243907059705151, 8.999999999999992895 ) ) ;
#18871 = ORIENTED_EDGE ( 'NONE', *, *, #6419, .T. ) ;
#18872 = ORIENTED_EDGE ( 'NONE', *, *, #16501, .F. ) ;
#18873 = AXIS2_PLACEMENT_3D ( 'NONE', #8554, #2529, #24496 ) ;
#18874 = ORIENTED_EDGE ( 'NONE', *, *, #6339, .F. ) ;
#18875 = CARTESIAN_POINT ( 'NONE',  ( 0.000000000000000000, 0.000000000000000000, 1.000000000000000000 ) ) ;
#18876 = ORIENTED_EDGE ( 'NONE', *, *, #5399, .F. ) ;
#18877 = CARTESIAN_POINT ( 'NONE',  ( 1.878215178124995832, -26.75312499938548783, 5.746835883940462963 ) ) ;
#18878 = ORIENTED_EDGE ( 'NONE', *, *, #3818, .T. ) ;
#18879 = FACE_OUTER_BOUND ( 'NONE', #3552, .T. ) ;
#18880 = AXIS2_PLACEMENT_3D ( 'NONE', #5199, #5447, #3490 ) ;
#18881 = AXIS2_PLACEMENT_3D ( 'NONE', #25663, #17314, #7480 ) ;
#18882 = ORIENTED_EDGE ( 'NONE', *, *, #8296, .F. ) ;
#18883 = CYLINDRICAL_SURFACE ( 'NONE', #10989, 0.5000000000000004441 ) ;
#18884 = CARTESIAN_POINT ( 'NONE',  ( -3.756430356249996994, 29.41562499938548569, 8.999999999999992895 ) ) ;
#18885 = FACE_OUTER_BOUND ( 'NONE', #10777, .T. ) ;
#18886 = EDGE_CURVE ( 'NONE', #16594, #3917, #20193, .T. ) ;
#18887 = CARTESIAN_POINT ( 'NONE',  ( -1.071796769724490117, 26.48259618943233562, 4.999999999999992895 ) ) ;
#18888 = CARTESIAN_POINT ( 'NONE',  ( 18.71181319714904490, 18.71181319714897384, 4.999999999999991118 ) ) ;
#18889 = CARTESIAN_POINT ( 'NONE',  ( 19.52719570377026415, 19.52719570377018599, 4.662447845253954171 ) ) ;
#18890 = CYLINDRICAL_SURFACE ( 'NONE', #9626, 4.000000000000000000 ) ;
#18891 = EDGE_CURVE ( 'NONE', #23645, #9327, #17783, .T. ) ;
#18892 =( BOUNDED_CURVE ( )  B_SPLINE_CURVE ( 2, ( #5396, #9335, #10888, #19389, #13000, #19126, #20980, #5273, #1359 ),
 .UNSPECIFIED., .F., .F. ) 
 B_SPLINE_CURVE_WITH_KNOTS ( ( 3, 2, 2, 2, 3 ),
 ( 0.2750000000000000222, 0.2833333333333333259, 0.2999999999999999889, 0.3166666666666666519, 0.3250000000000000111 ),
 .UNSPECIFIED. ) 
 CURVE ( )  GEOMETRIC_REPRESENTATION_ITEM ( )  RATIONAL_B_SPLINE_CURVE ( ( 0.9330127018922194093, 0.9330127018922196314, 1.000000000000000000, 0.8660254037844387076, 1.000000000000000000, 0.8660254037844387076, 1.000000000000000000, 0.9330127018922191873, 0.9330127018922194093 ) ) 
 REPRESENTATION_ITEM ( '' )  );
#18893 = CARTESIAN_POINT ( 'NONE',  ( 3.735045420075836212E-15, 27.95312499938548001, 4.662447845253954171 ) ) ;
#18894 = AXIS2_PLACEMENT_3D ( 'NONE', #5335, #13318, #23380 ) ;
#18895 = AXIS2_PLACEMENT_3D ( 'NONE', #10580, #10313, #18307 ) ;
#18896 = CARTESIAN_POINT ( 'NONE',  ( 18.22561351908507277, 20.88181089704437454, 5.746835883940462963 ) ) ;
#18897 = CARTESIAN_POINT ( 'NONE',  ( 0.000000000000000000, 0.000000000000000000, -6.500000000000000000 ) ) ;
#18898 = ORIENTED_EDGE ( 'NONE', *, *, #22465, .F. ) ;
#18899 = EDGE_CURVE ( 'NONE', #11588, #24788, #67, .T. ) ;
#18900 = CARTESIAN_POINT ( 'NONE',  ( 2.000000000000005329, 25.46874999877096712, 5.535898384862238508 ) ) ;
#18901 = CARTESIAN_POINT ( 'NONE',  ( 3.756430356249996105, -27.57812499938548356, 6.831223922626973533 ) ) ;
#18902 = FACE_OUTER_BOUND ( 'NONE', #3115, .T. ) ;
#18903 = CARTESIAN_POINT ( 'NONE',  ( 2.620986760973688460E-15, 29.33124999877096784, 13.61880215351699874 ) ) ;
#18904 = CARTESIAN_POINT ( 'NONE',  ( 1.152368580279349075, 29.97923206407486774, 12.84165680230635509 ) ) ;
#18906 = ORIENTED_EDGE ( 'NONE', *, *, #17987, .T. ) ;
#18905 = DIRECTION ( 'NONE',  ( 1.000000000000000000, 0.000000000000000000, 0.000000000000000000 ) ) ;
#18907 = ORIENTED_EDGE ( 'NONE', *, *, #24716, .T. ) ;
#18908 = CARTESIAN_POINT ( 'NONE',  ( -30.60000000000000142, 3.257552089140643357E-13, -6.500000000000000000 ) ) ;
#18909 = CARTESIAN_POINT ( 'NONE',  ( -0.5000000000000000000, 0.8660254037844387076, 19.50000000000000000 ) ) ;
#18910 = VERTEX_POINT ( 'NONE', #25651 ) ;
#18911 = EDGE_CURVE ( 'NONE', #22249, #18179, #2037, .T. ) ;
#18912 = CARTESIAN_POINT ( 'NONE',  ( 1.878215178124998497, -29.60312499938548569, 12.25316411605951927 ) ) ;
#18913 = CARTESIAN_POINT ( 'NONE',  ( -3.469446951953614189E-15, -30.00000000000000355, 8.999999999999992895 ) ) ;
#18914 = VECTOR ( 'NONE', #18314, 1000.000000000000000 ) ;
#18915 = CARTESIAN_POINT ( 'NONE',  ( 19.50730832598392084, 19.50730832598383913, 12.99999999999999289 ) ) ;
#18916 = CARTESIAN_POINT ( 'NONE',  ( -2.000000000000000000, 25.30000000000001137, 12.46410161513774639 ) ) ;
#18917 = VECTOR ( 'NONE', #5271, 1000.000000000000000 ) ;
#18918 = CARTESIAN_POINT ( 'NONE',  ( 2.000000000000000000, 25.37500000000000355, 12.46410161513774817 ) ) ;
#18919 = DIRECTION ( 'NONE',  ( 1.000000000000000000, 0.000000000000000000, 0.000000000000000000 ) ) ;
#18920 = EDGE_CURVE ( 'NONE', #16889, #14283, #17419, .T. ) ;
#18921 = CYLINDRICAL_SURFACE ( 'NONE', #19605, 0.5000000000000004441 ) ;
#18922 = DIRECTION ( 'NONE',  ( 0.8763066800438685799, 0.4817536741017063306, 0.000000000000000000 ) ) ;
#18923 = AXIS2_PLACEMENT_3D ( 'NONE', #18151, #5975, #7932 ) ;
#18924 = CARTESIAN_POINT ( 'NONE',  ( -3.756430356249997438, 26.30312499938548854, 11.16877607737301048 ) ) ;
#18925 = CARTESIAN_POINT ( 'NONE',  ( -1.626862140677534194E-14, -28.43124999877096570, 12.99999999999999289 ) ) ;
#18926 = CARTESIAN_POINT ( 'NONE',  ( 16.36952198446861217, 19.19794910921473630, 5.535898384862237620 ) ) ;
#18927 = CARTESIAN_POINT ( 'NONE',  ( 18.89079960070236908, 18.89079960070229802, 4.662447845253954171 ) ) ;
#18928 = EDGE_CURVE ( 'NONE', #523, #20603, #3417, .T. ) ;
#18929 = DIRECTION ( 'NONE',  ( -0.000000000000000000, -0.000000000000000000, -1.000000000000000000 ) ) ;
#18930 = CARTESIAN_POINT ( 'NONE',  ( -1.878215178124995832, 28.89062499938548356, 5.746835883940462963 ) ) ;
#18931 = EDGE_CURVE ( 'NONE', #9061, #21831, #5380, .T. ) ;
#18932 = CARTESIAN_POINT ( 'NONE',  ( 23.85222316637486273, 18.19536891688240843, 8.999999999999992895 ) ) ;
#18933 = CARTESIAN_POINT ( 'NONE',  ( 19.60674521665374215, 19.60674521665367465, 13.33755215474603162 ) ) ;
#18934 = CARTESIAN_POINT ( 'NONE',  ( 22.32573188046920265, 21.65113613650335367, -2.750000000000000000 ) ) ;
#18935 = ORIENTED_EDGE ( 'NONE', *, *, #21610, .T. ) ;
#18936 = CARTESIAN_POINT ( 'NONE',  ( -1.999999999999998224, 28.90000000000000213, 12.46410161513774639 ) ) ;
#18937 = CARTESIAN_POINT ( 'NONE',  ( -3.999999999999997335, 27.45624999877096784, 11.30940107675849404 ) ) ;
#18938 = CARTESIAN_POINT ( 'NONE',  ( -1.878215178125000939, -29.11562499938548498, 12.25316411605952283 ) ) ;
#18940 = ORIENTED_EDGE ( 'NONE', *, *, #21461, .F. ) ;
#18939 = DIRECTION ( 'NONE',  ( 0.6374239897486886353, -0.7705132427757902525, 0.000000000000000000 ) ) ;
#18941 = CARTESIAN_POINT ( 'NONE',  ( 24.86329371854768766, -18.68225429291730677, 1.000000000000000000 ) ) ;
#18942 =( BOUNDED_CURVE ( )  B_SPLINE_CURVE ( 2, ( #24898, #18887, #7364, #1482, #1219, #14956, #14836, #11145, #3059 ),
 .UNSPECIFIED., .F., .F. ) 
 B_SPLINE_CURVE_WITH_KNOTS ( ( 3, 2, 2, 2, 3 ),
 ( 0.3250000000000000111, 0.3333333333333333148, 0.3499999999999999778, 0.3666666666666666408, 0.3750000000000000000 ),
 .UNSPECIFIED. ) 
 CURVE ( )  GEOMETRIC_REPRESENTATION_ITEM ( )  RATIONAL_B_SPLINE_CURVE ( ( 0.9330127018922194093, 0.9330127018922196314, 1.000000000000000000, 0.8660254037844387076, 1.000000000000000000, 0.8660254037844387076, 1.000000000000000000, 0.9330127018922194093, 0.9330127018922194093 ) ) 
 REPRESENTATION_ITEM ( '' )  );
#18943 = ORIENTED_EDGE ( 'NONE', *, *, #21358, .T. ) ;
#18944 = CARTESIAN_POINT ( 'NONE',  ( -3.735045420075836212E-15, -27.05312499938548498, 4.662447845253954171 ) ) ;
#18945 = ORIENTED_EDGE ( 'NONE', *, *, #13664, .T. ) ;
#18946 = EDGE_LOOP ( 'NONE', ( #17370, #12260, #18325, #2038 ) ) ;
#18947 = CARTESIAN_POINT ( 'NONE',  ( -3.756430356249998326, 28.66562499938548925, 11.16877607737301226 ) ) ;
#18948 = CYLINDRICAL_SURFACE ( 'NONE', #20615, 0.5000000000000004441 ) ;
#18949 = CARTESIAN_POINT ( 'NONE',  ( -1.878215178124995832, -5.746835883940462963, 4.453124999385483562 ) ) ;
#18950 =( NAMED_UNIT ( * ) PLANE_ANGLE_UNIT ( ) SI_UNIT ( $, .RADIAN. ) );
#18951 = CARTESIAN_POINT ( 'NONE',  ( -3.163547630074431627, 38.99403850649169812, 4.493343988836014269 ) ) ;
#18952 = CARTESIAN_POINT ( 'NONE',  ( 1.878215178125004048, 27.46562499938548640, 5.746835883940462963 ) ) ;
#18953 = CARTESIAN_POINT ( 'NONE',  ( 16.23990935651717393, 26.52310962334745170, -2.750000000000000000 ) ) ;
#18954 = CARTESIAN_POINT ( 'NONE',  ( 3.999999999999995559, -28.78750000000000142, 6.690598923241487306 ) ) ;
#18955 = CARTESIAN_POINT ( 'NONE',  ( -1.878215178124995832, 28.89062499938548356, 5.746835883940462963 ) ) ;
#18956 = CYLINDRICAL_SURFACE ( 'NONE', #21245, 0.5000000000000004441 ) ;
#18957 = LINE ( 'NONE', #5342, #10108 ) ;
#18958 = ADVANCED_FACE ( 'NONE', ( #2937 ), #19621, .T. ) ;
#18959 = DIRECTION ( 'NONE',  ( -0.000000000000000000, -0.000000000000000000, 1.000000000000000000 ) ) ;
#18960 = CARTESIAN_POINT ( 'NONE',  ( -1.878215178125004048, -28.02812499938548640, 5.746835883940462963 ) ) ;
#18961 = CARTESIAN_POINT ( 'NONE',  ( 17.16943652981684210, 22.82629077930915074, 6.690598923241487306 ) ) ;
#18962 = EDGE_CURVE ( 'NONE', #8071, #19049, #18746, .T. ) ;
#18963 = DIRECTION ( 'NONE',  ( 1.000000000000000000, 0.000000000000000000, 0.000000000000000000 ) ) ;
#18964 = AXIS2_PLACEMENT_3D ( 'NONE', #5299, #13418, #11171 ) ;
#18965 = CARTESIAN_POINT ( 'NONE',  ( 29.09636799667083906, 10.98232076577211558, -2.750000000000000000 ) ) ;
#18966 = CARTESIAN_POINT ( 'NONE',  ( 2.642157743709451889, -29.88401080970086099, 12.01472878375391140 ) ) ;
#18967 = VERTEX_POINT ( 'NONE', #4894 ) ;
#18968 = LINE ( 'NONE', #10985, #3325 ) ;
#18970 = ORIENTED_EDGE ( 'NONE', *, *, #2052, .F. ) ;
#18969 = CARTESIAN_POINT ( 'NONE',  ( -14.98253926456356666, -27.25313774936403988, -6.500000000000000000 ) ) ;
#18971 = EDGE_CURVE ( 'NONE', #17747, #4816, #16231, .T. ) ;
#18972 = VERTEX_POINT ( 'NONE', #12870 ) ;
#18973 = ORIENTED_EDGE ( 'NONE', *, *, #5637, .T. ) ;
#18974 = ORIENTED_EDGE ( 'NONE', *, *, #23256, .T. ) ;
#18975 = ORIENTED_EDGE ( 'NONE', *, *, #18861, .F. ) ;
#18976 = CYLINDRICAL_SURFACE ( 'NONE', #16809, 4.000000000000000000 ) ;
#18977 = VERTEX_POINT ( 'NONE', #9809 ) ;
#18978 = ORIENTED_EDGE ( 'NONE', *, *, #11349, .T. ) ;
#18979 = CARTESIAN_POINT ( 'NONE',  ( 3.756430356250002323, 28.81562499938548427, 11.16877607737301403 ) ) ;
#18980 = CARTESIAN_POINT ( 'NONE',  ( 2.672651547586948120E-15, -13.33755215474602984, 4.190624999385483385 ) ) ;
#18981 = CARTESIAN_POINT ( 'NONE',  ( 8.831537335106614961E-15, 27.13750000000000284, 12.99999999999999112 ) ) ;
#18982 = CARTESIAN_POINT ( 'NONE',  ( 20.72043839702256207, 20.72043839702248036, 4.662447845253954171 ) ) ;
#18983 = CARTESIAN_POINT ( 'NONE',  ( -3.756430356249997882, 26.86562499938548498, 11.16877607737301226 ) ) ;
#18984 = DIRECTION ( 'NONE',  ( 0.000000000000000000, 1.000000000000000000, 0.000000000000000000 ) ) ;
#18985 = CARTESIAN_POINT ( 'NONE',  ( -3.756430356249995661, -6.831223922626973533, 4.378124999385480720 ) ) ;
#18986 = CARTESIAN_POINT ( 'NONE',  ( 4.000000000000003553, -8.999999999999992895, 4.500000000000000888 ) ) ;
#18987 = FACE_OUTER_BOUND ( 'NONE', #3148, .T. ) ;
#18988 = CARTESIAN_POINT ( 'NONE',  ( -5.706339097770935176, 29.50000000000000000, 7.145898033750358813 ) ) ;
#18989 = EDGE_CURVE ( 'NONE', #4582, #25396, #9316, .T. ) ;
#18990 = CARTESIAN_POINT ( 'NONE',  ( 21.21320343559646915, 21.21320343559638744, 4.999999999999992006 ) ) ;
#18991 = CARTESIAN_POINT ( 'NONE',  ( -3.756430356249996105, -6.831223922626973533, 4.040624999385483918 ) ) ;
#18992 = ADVANCED_FACE ( 'NONE', ( #13503 ), #21474, .T. ) ;
#18993 = DIRECTION ( 'NONE',  ( 1.000000000000000000, 0.000000000000000000, 0.000000000000000000 ) ) ;
#18994 = CARTESIAN_POINT ( 'NONE',  ( -2.000000000000003997, -25.52500000000000213, 5.535898384862238508 ) ) ;
#18995 = ORIENTED_EDGE ( 'NONE', *, *, #4870, .T. ) ;
#18996 = ORIENTED_EDGE ( 'NONE', *, *, #2120, .T. ) ;
#18997 = ORIENTED_EDGE ( 'NONE', *, *, #5292, .F. ) ;
#18998 = CARTESIAN_POINT ( 'NONE',  ( -28.14012133169333651, -13.24173596767349359, -6.500000000000000000 ) ) ;
#18999 = ORIENTED_EDGE ( 'NONE', *, *, #1740, .T. ) ;
#19000 = CARTESIAN_POINT ( 'NONE',  ( -3.756430356250002323, -26.56562499938548427, 11.16877607737301226 ) ) ;
#19001 = EDGE_LOOP ( 'NONE', ( #1562, #17899, #14826, #3914 ) ) ;
#19002 = DIRECTION ( 'NONE',  ( 1.000000000000000000, 0.000000000000000000, 0.000000000000000000 ) ) ;
#19003 = EDGE_CURVE ( 'NONE', #7580, #18031, #22915, .T. ) ;
#19004 = VERTEX_POINT ( 'NONE', #15591 ) ;
#19005 = CARTESIAN_POINT ( 'NONE',  ( -27.92360179968363809, 13.69242354489171554, 1.000000000000000000 ) ) ;
#19006 = CARTESIAN_POINT ( 'NONE',  ( 1.878215178125004048, 28.81562499938548427, 5.746835883940462963 ) ) ;
#19007 = DIRECTION ( 'NONE',  ( -0.9921147013144768767, 0.1253332335643120576, 0.000000000000000000 ) ) ;
#19008 = FACE_OUTER_BOUND ( 'NONE', #11338, .T. ) ;
#19009 = CARTESIAN_POINT ( 'NONE',  ( 17.67766952966372429, 17.67766952966365679, 8.999999999999992895 ) ) ;
#19010 = CARTESIAN_POINT ( 'NONE',  ( 19.44991966514168169, 16.79372228718224491, 12.25316411605952283 ) ) ;
#19011 = CARTESIAN_POINT ( 'NONE',  ( 0.000000000000000000, 0.000000000000000000, -6.500000000000000000 ) ) ;
#19012 = CARTESIAN_POINT ( 'NONE',  ( 1.878215178125004048, 29.26562499938548356, 5.746835883940462963 ) ) ;
#19013 = CARTESIAN_POINT ( 'NONE',  ( 17.24222938593383248, 22.55462414185250353, 6.831223922626973533 ) ) ;
#19014 = LINE ( 'NONE', #23195, #9921 ) ;
#19015 = EDGE_LOOP ( 'NONE', ( #20799, #6421, #8036, #3068 ) ) ;
#19016 = CARTESIAN_POINT ( 'NONE',  ( -1.999999999999993117, 27.34374999877097068, 5.535898384862237620 ) ) ;
#19017 = CARTESIAN_POINT ( 'NONE',  ( -2.672651547586948120E-15, -27.27812499938548640, 13.33755215474603162 ) ) ;
#19018 = CIRCLE ( 'NONE', #20685, 31.10000000000000142 ) ;
#19019 = LINE ( 'NONE', #5286, #829 ) ;
#19020 = EDGE_CURVE ( 'NONE', #2372, #20735, #13622, .T. ) ;
#19021 = CARTESIAN_POINT ( 'NONE',  ( 3.756430356250004099, 26.64062499938549067, 6.831223922626973533 ) ) ;
#19022 = CARTESIAN_POINT ( 'NONE',  ( 3.469446951953614189E-15, 30.00000000000000355, 4.999999999999992006 ) ) ;
#19024 = ORIENTED_EDGE ( 'NONE', *, *, #11490, .T. ) ;
#19023 = CARTESIAN_POINT ( 'NONE',  ( 3.735045420075836212E-15, -4.662447845253954171, 0.2531249993854848279 ) ) ;
#19025 = VERTEX_POINT ( 'NONE', #9700 ) ;
#19026 = CARTESIAN_POINT ( 'NONE',  ( 3.469446951953614189E-15, 30.00000000000000355, 8.999999999999992895 ) ) ;
#19027 = CARTESIAN_POINT ( 'NONE',  ( 3.469446951953614189E-15, 40.00000000000000000, 8.999999999999992895 ) ) ;
#19028 = ORIENTED_EDGE ( 'NONE', *, *, #21994, .T. ) ;
#19029 = CARTESIAN_POINT ( 'NONE',  ( 1.878215178124995832, -28.55312499938548498, 5.746835883940462963 ) ) ;
#19030 = EDGE_CURVE ( 'NONE', #12924, #6983, #17683, .T. ) ;
#19031 = CARTESIAN_POINT ( 'NONE',  ( -5.532151103383212032, 31.50000000000000000, 11.32277940608570432 ) ) ;
#19032 = CARTESIAN_POINT ( 'NONE',  ( 3.756430356250000546, 25.55312499938548854, 11.16877607737301403 ) ) ;
#19033 = AXIS2_PLACEMENT_3D ( 'NONE', #588, #11115, #24497 ) ;
#19034 = CARTESIAN_POINT ( 'NONE',  ( 20.27939324173355473, 18.76364371388142516, 12.99999999999998757 ) ) ;
#19035 = CARTESIAN_POINT ( 'NONE',  ( 3.756430356250004543, 28.70312499938549067, 11.16877607737301226 ) ) ;
#19036 = DIRECTION ( 'NONE',  ( 0.000000000000000000, 1.000000000000000000, 0.000000000000000000 ) ) ;
#19037 = APPLICATION_PROTOCOL_DEFINITION ( 'draft international standard', 'automotive_design', 1998, #24801 ) ;
#19038 = DIRECTION ( 'NONE',  ( -0.5877852522924652545, 0.8090169943749532244, 0.000000000000000000 ) ) ;
#19039 = CARTESIAN_POINT ( 'NONE',  ( -27.10000000000000497, 0.6000000000000000888, 19.59999999999999787 ) ) ;
#19040 = CARTESIAN_POINT ( 'NONE',  ( -1.878215178124998497, 26.34062499938548285, 12.25316411605951927 ) ) ;
#19041 = CARTESIAN_POINT ( 'NONE',  ( 10.98232076577200722, -29.09636799667087459, -6.500000000000000000 ) ) ;
#19042 = CARTESIAN_POINT ( 'NONE',  ( 19.14491610062580662, 16.31648897587954750, 5.535898384862238508 ) ) ;
#19043 = CARTESIAN_POINT ( 'NONE',  ( 18.17706369300767832, 23.83391794249997986, 11.30940107675849404 ) ) ;
#19044 = FACE_OUTER_BOUND ( 'NONE', #3020, .T. ) ;
#19045 = CARTESIAN_POINT ( 'NONE',  ( 3.756430356250003655, 27.39062499938548356, 8.999999999999992895 ) ) ;
#19046 = CARTESIAN_POINT ( 'NONE',  ( -30.91344420362550593, -3.401318489840770454, -2.750000000000000000 ) ) ;
#19047 = CARTESIAN_POINT ( 'NONE',  ( 17.50966790313369259, 20.16586528109299437, 5.746835883940462963 ) ) ;
#19048 = LINE ( 'NONE', #18934, #15889 ) ;
#19049 = VERTEX_POINT ( 'NONE', #17926 ) ;
#19050 = DIRECTION ( 'NONE',  ( -0.000000000000000000, -0.000000000000000000, 1.000000000000000000 ) ) ;
#19051 = CARTESIAN_POINT ( 'NONE',  ( -3.999999999999996447, 26.96874999877096712, 8.999999999999992895 ) ) ;
#19052 = CARTESIAN_POINT ( 'NONE',  ( -3.756430356250002323, -28.70312499938548356, 11.16877607737301226 ) ) ;
#19054 = ORIENTED_EDGE ( 'NONE', *, *, #19386, .T. ) ;
#19053 = CYLINDRICAL_SURFACE ( 'NONE', #23792, 0.5000000000000004441 ) ;
#19055 = CARTESIAN_POINT ( 'NONE',  ( -3.756430356249996105, 25.89062499938548356, 6.831223922626973533 ) ) ;
#19056 = EDGE_CURVE ( 'NONE', #13467, #16526, #12423, .T. ) ;
#19057 = ORIENTED_EDGE ( 'NONE', *, *, #17934, .T. ) ;
#19058 = CARTESIAN_POINT ( 'NONE',  ( -3.756430356250002323, -27.35312499938547859, 11.16877607737301226 ) ) ;
#19059 = ORIENTED_EDGE ( 'NONE', *, *, #19094, .T. ) ;
#19060 = PRODUCT_DEFINITION_SHAPE ( 'NONE', 'NONE',  #25882 ) ;
#19061 = EDGE_LOOP ( 'NONE', ( #10292, #12000, #1769, #2395, #5618, #13177 ) ) ;
#19062 = EDGE_CURVE ( 'NONE', #21186, #7772, #22429, .T. ) ;
#19063 = CARTESIAN_POINT ( 'NONE',  ( 19.92282844591920110, 22.43077534314094379, 12.59496732558994125 ) ) ;
#19064 = CARTESIAN_POINT ( 'NONE',  ( 3.756430356250003211, 27.05312499938548854, 8.999999999999992895 ) ) ;
#19065 = CARTESIAN_POINT ( 'NONE',  ( 2.672651547586948120E-15, -13.33755215474603162, 0.4781249993854826963 ) ) ;
#19066 = EDGE_CURVE ( 'NONE', #2564, #184, #17491, .T. ) ;
#19067 = CARTESIAN_POINT ( 'NONE',  ( 3.756430356250004099, -6.831223922626973533, 3.890624999385483562 ) ) ;
#19068 =( LENGTH_UNIT ( ) NAMED_UNIT ( * ) SI_UNIT ( .MILLI., .METRE. ) );
#19069 = CYLINDRICAL_SURFACE ( 'NONE', #17644, 4.000000000000000000 ) ;
#19070 = CARTESIAN_POINT ( 'NONE',  ( -3.756430356249995661, 29.37812499938548427, 6.831223922626973533 ) ) ;
#19071 = CARTESIAN_POINT ( 'NONE',  ( -1.022599059854450137E-14, 29.16250000000000497, 4.999999999999992006 ) ) ;
#19072 = DIRECTION ( 'NONE',  ( 0.000000000000000000, 0.000000000000000000, -1.000000000000000000 ) ) ;
#19073 = CARTESIAN_POINT ( 'NONE',  ( -1.878215178124995832, 29.34062499938548285, 5.746835883940462963 ) ) ;
#19074 = DIRECTION ( 'NONE',  ( 1.000000000000000000, 0.000000000000000000, 0.000000000000000000 ) ) ;
#19075 = DIRECTION ( 'NONE',  ( 0.6374239897486995154, 0.7705132427757811486, 0.000000000000000000 ) ) ;
#19076 = DIRECTION ( 'NONE',  ( 0.000000000000000000, 0.000000000000000000, 1.000000000000000000 ) ) ;
#19077 = DIRECTION ( 'NONE',  ( 0.000000000000000000, 0.000000000000000000, 1.000000000000000000 ) ) ;
#19078 = CARTESIAN_POINT ( 'NONE',  ( -1.878215178125004048, -27.57812499938548711, 5.746835883940462963 ) ) ;
#19079 =( BOUNDED_CURVE ( )  B_SPLINE_CURVE ( 2, ( #8128, #21592, #23948, #10200, #21982, #4057, #23681, #20144, #9703 ),
 .UNSPECIFIED., .F., .F. ) 
 B_SPLINE_CURVE_WITH_KNOTS ( ( 3, 2, 2, 2, 3 ),
 ( 0.7750000000000000222, 0.7833333333333333259, 0.8000000000000000444, 0.8166666666666666519, 0.8250000000000000666 ),
 .UNSPECIFIED. ) 
 CURVE ( )  GEOMETRIC_REPRESENTATION_ITEM ( )  RATIONAL_B_SPLINE_CURVE ( ( 0.9330127018922194093, 0.9330127018922194093, 1.000000000000000000, 0.8660254037844387076, 1.000000000000000000, 0.8660254037844387076, 1.000000000000000000, 0.9330127018922189652, 0.9330127018922194093 ) ) 
 REPRESENTATION_ITEM ( '' )  );
#19080 = CARTESIAN_POINT ( 'NONE',  ( -3.756430356249995661, 26.34062499938548285, 6.831223922626973533 ) ) ;
#19081 = CYLINDRICAL_SURFACE ( 'NONE', #15398, 4.000000000000000000 ) ;
#19082 = CARTESIAN_POINT ( 'NONE',  ( 0.000000000000000000, 0.000000000000000000, -6.500000000000000000 ) ) ;
#19083 = CARTESIAN_POINT ( 'NONE',  ( 3.469446951953614189E-15, 40.00000000000000000, 4.999999999999992006 ) ) ;
#19084 = VERTEX_POINT ( 'NONE', #20140 ) ;
#19085 = DIRECTION ( 'NONE',  ( 0.000000000000000000, 0.000000000000000000, 1.000000000000000000 ) ) ;
#19087 = ORIENTED_EDGE ( 'NONE', *, *, #15996, .T. ) ;
#19086 = DIRECTION ( 'NONE',  ( 0.000000000000000000, -0.000000000000000000, 1.000000000000000000 ) ) ;
#19088 = ORIENTED_EDGE ( 'NONE', *, *, #3092, .T. ) ;
#19089 = ORIENTED_EDGE ( 'NONE', *, *, #18173, .T. ) ;
#19090 = ORIENTED_EDGE ( 'NONE', *, *, #14693, .F. ) ;
#19091 = ORIENTED_EDGE ( 'NONE', *, *, #23124, .T. ) ;
#19092 = CARTESIAN_POINT ( 'NONE',  ( 0.000000000000000000, 0.000000000000000000, -6.500000000000000000 ) ) ;
#19093 = FACE_OUTER_BOUND ( 'NONE', #21037, .T. ) ;
#19094 = EDGE_CURVE ( 'NONE', #24890, #20539, #20836, .T. ) ;
#19095 = CARTESIAN_POINT ( 'NONE',  ( 2.672651547586948120E-15, 27.84062499938548640, 13.33755215474603162 ) ) ;
#19096 = EDGE_CURVE ( 'NONE', #2372, #20798, #9755, .T. ) ;
#19097 = CARTESIAN_POINT ( 'NONE',  ( -3.756430356249995661, -6.831223922626973533, 4.040624999385483918 ) ) ;
#19098 = CARTESIAN_POINT ( 'NONE',  ( -3.999999999999996003, -6.690598923241487306, 1.931249998770966814 ) ) ;
#19099 = CARTESIAN_POINT ( 'NONE',  ( 4.000000000000003553, 29.50000000000000355, 8.999999999999992895 ) ) ;
#19100 = CARTESIAN_POINT ( 'NONE',  ( 3.756430356250003655, 27.05312499938548498, 8.999999999999992895 ) ) ;
#19101 = CARTESIAN_POINT ( 'NONE',  ( 26.00000000000000355, 1.592040838891558898E-15, 20.00000599999999906 ) ) ;
#19102 = CARTESIAN_POINT ( 'NONE',  ( 30.63887302793244061, -5.335677986744896906, -2.750000000000000000 ) ) ;
#19103 = CARTESIAN_POINT ( 'NONE',  ( 2.672651547586948120E-15, -13.33755215474602984, 4.078124999385480010 ) ) ;
#19104 = CARTESIAN_POINT ( 'NONE',  ( -30.85476721088030061, -3.897863563849544466, -6.500000000000000000 ) ) ;
#19105 = CARTESIAN_POINT ( 'NONE',  ( 3.756430356250003655, -8.999999999999992895, 4.753124999385485161 ) ) ;
#19106 = DIRECTION ( 'NONE',  ( 0.9510565162951541973, -0.3090169943749456194, 0.000000000000000000 ) ) ;
#19107 = DIRECTION ( 'NONE',  ( -0.7071067811865487940, -0.7071067811865463515, 0.000000000000000000 ) ) ;
#19108 = CARTESIAN_POINT ( 'NONE',  ( 4.000000000000003553, -8.999999999999992895, 0.3937499987709675020 ) ) ;
#19109 = DIRECTION ( 'NONE',  ( 1.000000000000000000, 0.000000000000000000, 0.000000000000000000 ) ) ;
#19110 = CARTESIAN_POINT ( 'NONE',  ( -4.000000000000003553, -25.48750000000000071, 6.690598923241489970 ) ) ;
#19111 = ORIENTED_EDGE ( 'NONE', *, *, #17910, .T. ) ;
#19112 = EDGE_LOOP ( 'NONE', ( #22035, #5008, #24857, #11113 ) ) ;
#19113 = ORIENTED_EDGE ( 'NONE', *, *, #15329, .T. ) ;
#19114 = DIRECTION ( 'NONE',  ( 1.000000000000000000, 0.000000000000000000, 0.000000000000000000 ) ) ;
#19115 = ORIENTED_EDGE ( 'NONE', *, *, #24563, .F. ) ;
#19116 = CARTESIAN_POINT ( 'NONE',  ( -1.878215178125000939, -26.52812499938548285, 12.25316411605952283 ) ) ;
#19117 = ORIENTED_EDGE ( 'NONE', *, *, #12094, .F. ) ;
#19118 = CARTESIAN_POINT ( 'NONE',  ( -1.999999999999998224, 28.90000000000000213, 12.46410161513774639 ) ) ;
#19119 = ADVANCED_FACE ( 'NONE', ( #17804 ), #7851, .F. ) ;
#19120 = ORIENTED_EDGE ( 'NONE', *, *, #10621, .F. ) ;
#19121 = CARTESIAN_POINT ( 'NONE',  ( 18.03564233677035489, 18.03564233677029094, 4.999999999999992006 ) ) ;
#19122 = CARTESIAN_POINT ( 'NONE',  ( -1.878215178124998497, 29.49062499938548498, 12.25316411605951927 ) ) ;
#19123 = CARTESIAN_POINT ( 'NONE',  ( 18.41702535870033941, 19.93277488655231267, 12.99999999999999467 ) ) ;
#19124 = EDGE_CURVE ( 'NONE', #10526, #3018, #18760, .T. ) ;
#19125 = CIRCLE ( 'NONE', #20369, 0.7500000000000001110 ) ;
#19126 = CARTESIAN_POINT ( 'NONE',  ( 4.000000000000003553, 26.38750000000000284, 6.690598923241489970 ) ) ;
#19127 = CARTESIAN_POINT ( 'NONE',  ( -27.92360179968358125, 13.69242354489182922, -2.750000000000000000 ) ) ;
#19128 = CARTESIAN_POINT ( 'NONE',  ( 16.65886629145492748, 21.97126104737360919, 11.16877607737301226 ) ) ;
#19129 = CARTESIAN_POINT ( 'NONE',  ( 0.000000000000000000, 0.000000000000000000, -6.500000000000000000 ) ) ;
#19130 = AXIS2_PLACEMENT_3D ( 'NONE', #24995, #7462, #9171 ) ;
#19131 = CARTESIAN_POINT ( 'NONE',  ( -3.999999999999996003, 26.53750000000000142, 6.690598923241487306 ) ) ;
#19132 = EDGE_CURVE ( 'NONE', #962, #23712, #406, .T. ) ;
#19133 = CARTESIAN_POINT ( 'NONE',  ( 21.12273290994980712, 15.81033815403099574, 11.16877607737301403 ) ) ;
#19134 = CARTESIAN_POINT ( 'NONE',  ( 5.840899737312979845, 31.50000000000000000, 10.37254881831474052 ) ) ;
#19135 = ORIENTED_EDGE ( 'NONE', *, *, #21074, .F. ) ;
#19136 = ORIENTED_EDGE ( 'NONE', *, *, #13959, .T. ) ;
#19137 = CARTESIAN_POINT ( 'NONE',  ( 0.000000000000000000, 27.53124999877097423, 13.61880215351699874 ) ) ;
#19138 = LINE ( 'NONE', #10077, #24183 ) ;
#19139 = CIRCLE ( 'NONE', #18738, 31.10000000000000142 ) ;
#19140 = DIRECTION ( 'NONE',  ( 0.000000000000000000, 0.000000000000000000, -1.000000000000000000 ) ) ;
#19141 = CIRCLE ( 'NONE', #16655, 31.10000000000000142 ) ;
#19142 = CARTESIAN_POINT ( 'NONE',  ( 2.672651547586948120E-15, 26.94062499938548783, 13.33755215474602984 ) ) ;
#19143 = FACE_BOUND ( 'NONE', #16793, .T. ) ;
#19144 = ORIENTED_EDGE ( 'NONE', *, *, #11851, .F. ) ;
#19145 = ORIENTED_EDGE ( 'NONE', *, *, #20794, .F. ) ;
#19146 = CARTESIAN_POINT ( 'NONE',  ( -27.10000000000000497, 0.6000000000000000888, 19.59999999999999787 ) ) ;
#19147 = AXIS2_PLACEMENT_3D ( 'NONE', #18614, #20042, #20175 ) ;
#19148 = CARTESIAN_POINT ( 'NONE',  ( -26.75313774936397948, 14.98253926456367502, -6.500000000000000000 ) ) ;
#19149 = AXIS2_PLACEMENT_3D ( 'NONE', #20919, #9134, #19075 ) ;
#19150 = VERTEX_POINT ( 'NONE', #15716 ) ;
#19151 = CARTESIAN_POINT ( 'NONE',  ( 1.878215178124995832, -29.00312499938548427, 5.746835883940462963 ) ) ;
#19152 = CARTESIAN_POINT ( 'NONE',  ( 3.756430356250000546, 29.15312499938548996, 11.16877607737301226 ) ) ;
#19153 = DIRECTION ( 'NONE',  ( 1.000000000000000000, 0.000000000000000000, 0.000000000000000000 ) ) ;
#19154 = CARTESIAN_POINT ( 'NONE',  ( -4.000000000000003553, -26.29374999877096997, 8.999999999999992895 ) ) ;
#19155 = CARTESIAN_POINT ( 'NONE',  ( -4.000000000000000000, 25.67500000000000426, 8.999999999999992895 ) ) ;
#19156 = ADVANCED_FACE ( 'NONE', ( #4054 ), #21721, .F. ) ;
#19157 = VECTOR ( 'NONE', #7666, 1000.000000000000000 ) ;
#19158 = DIRECTION ( 'NONE',  ( -0.000000000000000000, -0.000000000000000000, 1.000000000000000000 ) ) ;
#19159 = VECTOR ( 'NONE', #13774, 1000.000000000000000 ) ;
#19160 = SHAPE_DEFINITION_REPRESENTATION ( #9838, #25031 ) ;
#19161 = DIRECTION ( 'NONE',  ( 0.000000000000000000, 0.000000000000000000, 1.000000000000000000 ) ) ;
#19162 = CARTESIAN_POINT ( 'NONE',  ( -16.16421332384646448, 26.25859848311288403, 1.000000000000000000 ) ) ;
#19163 = CARTESIAN_POINT ( 'NONE',  ( 1.878215178125004048, 26.11562499938548498, 5.746835883940462963 ) ) ;
#19164 = CARTESIAN_POINT ( 'NONE',  ( -3.974064950101062088, -29.73565934716929959, 8.475804415688518390 ) ) ;
#19165 = CARTESIAN_POINT ( 'NONE',  ( 21.11597625318330174, 15.45912200369085632, 11.30940107675849760 ) ) ;
#19166 = CARTESIAN_POINT ( 'NONE',  ( 15.35955758102464408, 20.67195233694332401, 8.999999999999992895 ) ) ;
#19167 = DIRECTION ( 'NONE',  ( 0.000000000000000000, 0.000000000000000000, 1.000000000000000000 ) ) ;
#19168 = CARTESIAN_POINT ( 'NONE',  ( -3.756430356249995661, 27.12812499938548427, 6.831223922626973533 ) ) ;
#19169 = CARTESIAN_POINT ( 'NONE',  ( -9.610428525061097460, -29.57785765677920509, -6.500000000000000000 ) ) ;
#19170 = CARTESIAN_POINT ( 'NONE',  ( 18.97034911358585418, 18.97034911358578668, 13.33755215474603162 ) ) ;
#19171 = ORIENTED_EDGE ( 'NONE', *, *, #15059, .T. ) ;
#19172 = CARTESIAN_POINT ( 'NONE',  ( 3.756430356250004099, 26.19062499938548783, 6.831223922626973533 ) ) ;
#19173 = CARTESIAN_POINT ( 'NONE',  ( 3.756430356249996994, -29.41562499938548569, 8.999999999999992895 ) ) ;
#19175 = ORIENTED_EDGE ( 'NONE', *, *, #3594, .F. ) ;
#19174 = FACE_OUTER_BOUND ( 'NONE', #23400, .T. ) ;
#19176 = CARTESIAN_POINT ( 'NONE',  ( 3.756430356250002323, 25.66562499938548569, 11.16877607737301403 ) ) ;
#19177 = AXIS2_PLACEMENT_3D ( 'NONE', #3392, #12952, #9025 ) ;
#19178 = ORIENTED_EDGE ( 'NONE', *, *, #4769, .T. ) ;
#19179 = CARTESIAN_POINT ( 'NONE',  ( -1.878215178125000939, -28.21562499938548640, 12.25316411605952283 ) ) ;
#19180 = ORIENTED_EDGE ( 'NONE', *, *, #20774, .F. ) ;
#19181 = VERTEX_POINT ( 'NONE', #20003 ) ;
#19182 = DIRECTION ( 'NONE',  ( -0.000000000000000000, 1.000000000000000000, 0.000000000000000000 ) ) ;
#19183 = CARTESIAN_POINT ( 'NONE',  ( 3.756430356250004543, 27.54062499938548925, 6.831223922626973533 ) ) ;
#19184 = CIRCLE ( 'NONE', #21692, 0.4999999999999986122 ) ;
#19185 = AXIS2_PLACEMENT_3D ( 'NONE', #3190, #23324, #21378 ) ;
#19186 = CARTESIAN_POINT ( 'NONE',  ( 2.672651547586948120E-15, -13.33755215474603162, 1.828124999385482008 ) ) ;
#19187 = ADVANCED_FACE ( 'NONE', ( #11906 ), #25770, .F. ) ;
#19188 = CIRCLE ( 'NONE', #11256, 31.10000000000000142 ) ;
#19189 = LINE ( 'NONE', #13317, #7498 ) ;
#19190 = CARTESIAN_POINT ( 'NONE',  ( -8.831537335106614961E-15, -27.13750000000000284, 12.99999999999999112 ) ) ;
#19191 = AXIS2_PLACEMENT_3D ( 'NONE', #12776, #20746, #21257 ) ;
#19192 = ADVANCED_FACE ( 'NONE', ( #7994 ), #15981, .T. ) ;
#19193 = CYLINDRICAL_SURFACE ( 'NONE', #10466, 4.000000000000000000 ) ;
#19194 = CIRCLE ( 'NONE', #2499, 0.4999999999999989453 ) ;
#19195 = FACE_OUTER_BOUND ( 'NONE', #6670, .T. ) ;
#19196 = CARTESIAN_POINT ( 'NONE',  ( 2.000000000000003997, 28.67500000000000426, 5.535898384862238508 ) ) ;
#19197 = LINE ( 'NONE', #21676, #4109 ) ;
#19198 = DIRECTION ( 'NONE',  ( 0.000000000000000000, 0.000000000000000000, -1.000000000000000000 ) ) ;
#19199 = CARTESIAN_POINT ( 'NONE',  ( -0.5000000000000001110, 10.00000000000000000, 13.00000000000000178 ) ) ;
#19200 = EDGE_CURVE ( 'NONE', #8252, #5263, #6536, .T. ) ;
#19201 = CARTESIAN_POINT ( 'NONE',  ( -5.327558883616270613, -30.54913349766217934, -6.500000000000000000 ) ) ;
#19202 = CARTESIAN_POINT ( 'NONE',  ( -1.878215178125004048, -28.92812499938548854, 5.746835883940462963 ) ) ;
#19203 = CARTESIAN_POINT ( 'NONE',  ( 17.19595303411133713, 22.85280728360364577, 8.999999999999992895 ) ) ;
#19204 = FACE_OUTER_BOUND ( 'NONE', #1886, .T. ) ;
#19205 = CARTESIAN_POINT ( 'NONE',  ( 0.000000000000000000, 0.000000000000000000, 1.000000000000000000 ) ) ;
#19206 = CARTESIAN_POINT ( 'NONE',  ( 2.007411586324088226, -29.93355017142139118, 12.46960170373642640 ) ) ;
#19207 = ORIENTED_EDGE ( 'NONE', *, *, #17953, .T. ) ;
#19208 = CARTESIAN_POINT ( 'NONE',  ( 2.000000000000000888, 27.17500000000000071, 12.46410161513774817 ) ) ;
#19209 = EDGE_CURVE ( 'NONE', #19467, #22219, #14178, .T. ) ;
#19210 = DIRECTION ( 'NONE',  ( -0.7071067811865487940, -0.7071067811865463515, 0.000000000000000000 ) ) ;
#19212 = ORIENTED_EDGE ( 'NONE', *, *, #6740, .F. ) ;
#19211 = CYLINDRICAL_SURFACE ( 'NONE', #15012, 4.000000000000000000 ) ;
#19213 = ORIENTED_EDGE ( 'NONE', *, *, #6636, .F. ) ;
#19214 = VECTOR ( 'NONE', #2943, 1000.000000000000000 ) ;
#19215 = VERTEX_POINT ( 'NONE', #924 ) ;
#19216 = ORIENTED_EDGE ( 'NONE', *, *, #7271, .F. ) ;
#19217 = ORIENTED_EDGE ( 'NONE', *, *, #4652, .F. ) ;
#19218 = DIRECTION ( 'NONE',  ( 0.000000000000000000, 0.000000000000000000, 1.000000000000000000 ) ) ;
#19219 = DIRECTION ( 'NONE',  ( 1.000000000000000000, -0.000000000000000000, -0.000000000000000000 ) ) ;
#19220 = AXIS2_PLACEMENT_3D ( 'NONE', #19129, #14839, #6979 ) ;
#19221 = LINE ( 'NONE', #1180, #2643 ) ;
#19222 = VECTOR ( 'NONE', #6828, 1000.000000000000000 ) ;
#19223 = CARTESIAN_POINT ( 'NONE',  ( 1.878215178125000939, -12.25316411605952283, 1.415624999385481253 ) ) ;
#19224 = CARTESIAN_POINT ( 'NONE',  ( -3.999999999999997335, -11.30940107675849404, 1.106249998770969301 ) ) ;
#19225 = CARTESIAN_POINT ( 'NONE',  ( 29.99470236596026496, -8.217531866531317064, -2.750000000000000000 ) ) ;
#19226 = CARTESIAN_POINT ( 'NONE',  ( 1.878215178125004048, 25.32812499938548356, 5.746835883940462963 ) ) ;
#19227 = CARTESIAN_POINT ( 'NONE',  ( -1.999999999999998224, -12.46410161513774639, 3.843749998770965792 ) ) ;
#19228 = CARTESIAN_POINT ( 'NONE',  ( 2.000000000000003997, 28.61874999877096926, 5.535898384862238508 ) ) ;
#19229 = AXIS2_PLACEMENT_3D ( 'NONE', #21472, #3546, #11519 ) ;
#19230 = CARTESIAN_POINT ( 'NONE',  ( -3.756430356249996994, -8.999999999999992895, 3.065624999385483385 ) ) ;
#19231 = CARTESIAN_POINT ( 'NONE',  ( -2.000000000000000888, -25.76874999877096784, 12.46410161513774817 ) ) ;
#19232 = DIRECTION ( 'NONE',  ( 1.000000000000000000, 0.000000000000000000, 0.000000000000000000 ) ) ;
#19233 = DIRECTION ( 'NONE',  ( 1.000000000000000000, 0.000000000000000000, 0.000000000000000000 ) ) ;
#19234 = EDGE_CURVE ( 'NONE', #9004, #13890, #20928, .T. ) ;
#19235 = CARTESIAN_POINT ( 'NONE',  ( -4.000000000000003553, -27.19374999877096855, 8.999999999999992895 ) ) ;
#19236 = AXIS2_PLACEMENT_3D ( 'NONE', #6920, #2863, #8897 ) ;
#19237 = FACE_OUTER_BOUND ( 'NONE', #21482, .T. ) ;
#19238 = AXIS2_PLACEMENT_3D ( 'NONE', #20522, #773, #2617 ) ;
#19239 = CARTESIAN_POINT ( 'NONE',  ( -1.071796769724487453, 25.31740381056767930, 12.99999999999999467 ) ) ;
#19240 = DIRECTION ( 'NONE',  ( 1.000000000000000000, 0.000000000000000000, 0.000000000000000000 ) ) ;
#19241 = CARTESIAN_POINT ( 'NONE',  ( 4.000000000000018652, -6.690598923241496188, 4.031249998770966236 ) ) ;
#19242 = ORIENTED_EDGE ( 'NONE', *, *, #17010, .T. ) ;
#19243 = EDGE_CURVE ( 'NONE', #24788, #4092, #18766, .T. ) ;
#19244 = DIRECTION ( 'NONE',  ( 0.000000000000000000, 0.000000000000000000, 1.000000000000000000 ) ) ;
#19245 = EDGE_LOOP ( 'NONE', ( #22794, #14317, #12796, #3522 ) ) ;
#19247 = EDGE_CURVE ( 'NONE', #2083, #23233, #20002, .T. ) ;
#19246 = VECTOR ( 'NONE', #4177, 1000.000000000000000 ) ;
#19248 = ORIENTED_EDGE ( 'NONE', *, *, #15704, .T. ) ;
#19249 = CARTESIAN_POINT ( 'NONE',  ( 23.01025686871646059, 20.92219106202042056, -6.500000000000000000 ) ) ;
#19250 = VERTEX_POINT ( 'NONE', #10981 ) ;
#19251 = CARTESIAN_POINT ( 'NONE',  ( -3.756430356250003655, -28.85312499938548569, 8.999999999999992895 ) ) ;
#19252 = ORIENTED_EDGE ( 'NONE', *, *, #2922, .F. ) ;
#19253 = CARTESIAN_POINT ( 'NONE',  ( 3.756430356250003655, 25.14062499938548356, 8.999999999999992895 ) ) ;
#19254 = AXIS2_PLACEMENT_3D ( 'NONE', #5017, #4885, #17434 ) ;
#19255 = ORIENTED_EDGE ( 'NONE', *, *, #22425, .F. ) ;
#19256 = CARTESIAN_POINT ( 'NONE',  ( 3.752267015613588906E-15, 26.91250000000000142, 4.381197846482986158 ) ) ;
#19257 = DIRECTION ( 'NONE',  ( -0.000000000000000000, -0.000000000000000000, 1.000000000000000000 ) ) ;
#19258 = VECTOR ( 'NONE', #16849, 1000.000000000000000 ) ;
#19259 = AXIS2_PLACEMENT_3D ( 'NONE', #357, #12506, #20481 ) ;
#19260 = DIRECTION ( 'NONE',  ( 0.000000000000000000, -1.000000000000000000, 0.000000000000000000 ) ) ;
#19261 = CARTESIAN_POINT ( 'NONE',  ( -27.25313774936397948, 14.98253926456367502, -6.500000000000000000 ) ) ;
#19262 = CARTESIAN_POINT ( 'NONE',  ( 19.36809667800328683, 19.36809667800321932, 13.33755215474602984 ) ) ;
#19263 = DIRECTION ( 'NONE',  ( 0.000000000000000000, 0.000000000000000000, 1.000000000000000000 ) ) ;
#19264 = CARTESIAN_POINT ( 'NONE',  ( -3.999999999999996447, 25.22500000000000142, 8.999999999999992895 ) ) ;
#19265 = CARTESIAN_POINT ( 'NONE',  ( 18.41350252340144422, 18.41350252340138383, 13.33755215474603162 ) ) ;
#19266 = DIRECTION ( 'NONE',  ( 0.000000000000000000, 0.000000000000000000, 1.000000000000000000 ) ) ;
#19267 = CIRCLE ( 'NONE', #17616, 31.10000000000000142 ) ;
#19268 = ORIENTED_EDGE ( 'NONE', *, *, #8732, .F. ) ;
#19269 = VERTEX_POINT ( 'NONE', #16367 ) ;
#19270 = CARTESIAN_POINT ( 'NONE',  ( -1.999999999999993117, 28.69374999877097210, 5.535898384862237620 ) ) ;
#19271 = AXIS2_PLACEMENT_3D ( 'NONE', #8994, #16711, #754 ) ;
#19273 = EDGE_CURVE ( 'NONE', #18617, #11292, #18337, .T. ) ;
#19272 = CARTESIAN_POINT ( 'NONE',  ( 1.878215178124995832, -28.89062499938548356, 5.746835883940462963 ) ) ;
#19274 = AXIS2_PLACEMENT_3D ( 'NONE', #25263, #10866, #5373 ) ;
#19275 = VERTEX_POINT ( 'NONE', #20532 ) ;
#19276 = DIRECTION ( 'NONE',  ( 0.000000000000000000, 0.000000000000000000, 1.000000000000000000 ) ) ;
#19277 = CARTESIAN_POINT ( 'NONE',  ( -3.756430356249996994, 27.72812499938548569, 8.999999999999992895 ) ) ;
#19278 = CARTESIAN_POINT ( 'NONE',  ( 3.063240906311874401, 29.84319947910909931, 11.57226653943512851 ) ) ;
#19279 = VERTEX_POINT ( 'NONE', #8759 ) ;
#19280 = VERTEX_POINT ( 'NONE', #8515 ) ;
#19281 = DIRECTION ( 'NONE',  ( 0.000000000000000000, 0.000000000000000000, 1.000000000000000000 ) ) ;
#19282 = CIRCLE ( 'NONE', #20979, 31.10000000000000142 ) ;
#19283 = CARTESIAN_POINT ( 'NONE',  ( -31.06601413805603329, -1.453535542772396605, 1.000000000000000000 ) ) ;
#19284 = ORIENTED_EDGE ( 'NONE', *, *, #4498, .T. ) ;
#19285 = CARTESIAN_POINT ( 'NONE',  ( 3.756430356249996994, -28.62812499938548427, 8.999999999999992895 ) ) ;
#19286 = DIRECTION ( 'NONE',  ( 1.000000000000000000, 0.000000000000000000, 0.000000000000000000 ) ) ;
#19287 = CARTESIAN_POINT ( 'NONE',  ( -3.756430356249997882, 27.20312499938549067, 11.16877607737301048 ) ) ;
#19288 = CIRCLE ( 'NONE', #7611, 0.5000000000000001110 ) ;
#19289 = LINE ( 'NONE', #19415, #4339 ) ;
#19290 = CARTESIAN_POINT ( 'NONE',  ( -1.878215178124996498, 28.89062499938548711, 5.746835883940462963 ) ) ;
#19291 = CIRCLE ( 'NONE', #5101, 0.5000000000000004441 ) ;
#19292 = CIRCLE ( 'NONE', #18895, 0.4999999999999997780 ) ;
#19293 = APPLICATION_CONTEXT ( 'automotive_design' ) ;
#19294 = SHAPE_DEFINITION_REPRESENTATION ( #1534, #16033 ) ;
#19295 = LINE ( 'NONE', #23342, #25454 ) ;
#19296 = CIRCLE ( 'NONE', #20137, 31.10000000000000142 ) ;
#19297 = FACE_OUTER_BOUND ( 'NONE', #8836, .T. ) ;
#19298 = CARTESIAN_POINT ( 'NONE',  ( -3.756430356249996994, 26.71562499938548285, 8.999999999999992895 ) ) ;
#19299 = DIRECTION ( 'NONE',  ( 0.000000000000000000, 0.000000000000000000, 1.000000000000000000 ) ) ;
#19300 = CARTESIAN_POINT ( 'NONE',  ( 22.68720666332504621, 17.37481190740622239, 6.831223922626973533 ) ) ;
#19301 = CARTESIAN_POINT ( 'NONE',  ( 17.26874589022832751, 22.58114064614699856, 8.999999999999992895 ) ) ;
#19302 = ADVANCED_FACE ( 'NONE', ( #2746 ), #16748, .F. ) ;
#19303 = CARTESIAN_POINT ( 'NONE',  ( -3.526711513754773986, 31.50000000000000000, 13.85410196624972201 ) ) ;
#19304 =( BOUNDED_CURVE ( )  B_SPLINE_CURVE ( 2, ( #695, #8274, #16256, #8411, #20417, #24368, #14546, #10737, #4222 ),
 .UNSPECIFIED., .F., .F. ) 
 B_SPLINE_CURVE_WITH_KNOTS ( ( 3, 2, 2, 2, 3 ),
 ( 0.6750000000000000444, 0.6833333333333333481, 0.6999999999999999556, 0.7166666666666666741, 0.7249999999999999778 ),
 .UNSPECIFIED. ) 
 CURVE ( )  GEOMETRIC_REPRESENTATION_ITEM ( )  RATIONAL_B_SPLINE_CURVE ( ( 0.9330127018922194093, 0.9330127018922198534, 1.000000000000000000, 0.8660254037844387076, 1.000000000000000000, 0.8660254037844387076, 1.000000000000000000, 0.9330127018922194093, 0.9330127018922194093 ) ) 
 REPRESENTATION_ITEM ( '' )  );
#19305 = CARTESIAN_POINT ( 'NONE',  ( 3.735045420075836212E-15, 28.40312499938548640, 4.662447845253954171 ) ) ;
#19307 = EDGE_CURVE ( 'NONE', #21795, #23357, #14994, .T. ) ;
#19306 = CARTESIAN_POINT ( 'NONE',  ( -3.999999999999996447, -8.999999999999992895, 2.868749998770965703 ) ) ;
#19308 = CIRCLE ( 'NONE', #10963, 6.000000000000000000 ) ;
#19309 = CARTESIAN_POINT ( 'NONE',  ( 16.23460222274299980, 21.54699697866167440, 8.999999999999992895 ) ) ;
#19310 = CARTESIAN_POINT ( 'NONE',  ( 4.000000000000003553, -8.999999999999992895, 3.149999999999999911 ) ) ;
#19311 = ORIENTED_EDGE ( 'NONE', *, *, #14571, .T. ) ;
#19312 = CARTESIAN_POINT ( 'NONE',  ( 2.620986760973688460E-15, 25.73124999877096997, 13.61880215351699874 ) ) ;
#19313 = CARTESIAN_POINT ( 'NONE',  ( 3.735045420075836212E-15, 25.36562499938548498, 4.662447845253954171 ) ) ;
#19314 = CARTESIAN_POINT ( 'NONE',  ( -2.000000000000003997, -25.07499999999999929, 5.535898384862238508 ) ) ;
#19316 = ORIENTED_EDGE ( 'NONE', *, *, #9208, .F. ) ;
#19315 = CARTESIAN_POINT ( 'NONE',  ( -1.878215178124994722, 25.40312499938548996, 5.746835883940462963 ) ) ;
#19317 = CARTESIAN_POINT ( 'NONE',  ( 2.672651547586948120E-15, 26.94062499938548783, 13.33755215474603162 ) ) ;
#19318 = EDGE_CURVE ( 'NONE', #19944, #10324, #24719, .T. ) ;
#19319 = CIRCLE ( 'NONE', #8048, 31.10000000000000142 ) ;
#19320 = ORIENTED_EDGE ( 'NONE', *, *, #22473, .F. ) ;
#19321 = CARTESIAN_POINT ( 'NONE',  ( -2.672651547586948120E-15, -27.27812499938548285, 13.33755215474602984 ) ) ;
#19322 = VERTEX_POINT ( 'NONE', #18834 ) ;
#19323 = VERTEX_POINT ( 'NONE', #14912 ) ;
#19324 = CARTESIAN_POINT ( 'NONE',  ( 3.526711513754818395, 31.50000000000000000, 4.145898033750289535 ) ) ;
#19325 = CARTESIAN_POINT ( 'NONE',  ( 4.006172263299091013E-15, 26.71562499938548996, 4.662447845253954171 ) ) ;
#19326 = ADVANCED_FACE ( 'NONE', ( #16887 ), #24333, .T. ) ;
#19327 = B_SPLINE_CURVE_WITH_KNOTS ( 'NONE', 3,
 ( #7951, #5858, #2207, #13975, #8089, #11874, #17766, #24293, #3903, #14368, #19841, #25735, #18033, #1942, #9904, #21944 ),
 .UNSPECIFIED., .F., .F.,
 ( 4, 2, 2, 2, 2, 2, 2, 4 ),
 ( 2.789812634921229689E-07, 0.0002085651107750574140, 0.0004168512402866226684, 0.0006251373697981880582, 0.0008334234993097532854, 0.001041709628821318621, 0.001249995758332883957, 0.001666568017356004870 ),
 .UNSPECIFIED. ) ;
#19328 = CARTESIAN_POINT ( 'NONE',  ( 3.735045420075836212E-15, -4.662447845253954171, 1.603124999385479921 ) ) ;
#19329 =( NAMED_UNIT ( * ) PLANE_ANGLE_UNIT ( ) SI_UNIT ( $, .RADIAN. ) );
#19330 = DIRECTION ( 'NONE',  ( 1.000000000000000000, 0.000000000000000000, 0.000000000000000000 ) ) ;
#19331 = CIRCLE ( 'NONE', #22689, 31.10000000000000142 ) ;
#19332 = DIRECTION ( 'NONE',  ( 1.000000000000000000, 0.000000000000000000, 0.000000000000000000 ) ) ;
#19333 = CYLINDRICAL_SURFACE ( 'NONE', #23446, 4.000000000000000000 ) ;
#19334 = DIRECTION ( 'NONE',  ( -0.000000000000000000, -0.000000000000000000, 1.000000000000000000 ) ) ;
#19335 = DIRECTION ( 'NONE',  ( -1.000000000000000000, 0.000000000000000000, 0.000000000000000000 ) ) ;
#19336 = DIRECTION ( 'NONE',  ( 0.000000000000000000, -0.000000000000000000, 1.000000000000000000 ) ) ;
#19337 = DIRECTION ( 'NONE',  ( 1.000000000000000000, 0.000000000000000000, 0.000000000000000000 ) ) ;
#19338 = VERTEX_POINT ( 'NONE', #10586 ) ;
#19339 = DIRECTION ( 'NONE',  ( 1.000000000000000000, 0.000000000000000000, 0.000000000000000000 ) ) ;
#19340 = LINE ( 'NONE', #9138, #15092 ) ;
#19341 = CARTESIAN_POINT ( 'NONE',  ( 1.878215178125004048, 25.32812499938548356, 5.746835883940462963 ) ) ;
#19342 = CARTESIAN_POINT ( 'NONE',  ( 0.000000000000000000, 0.000000000000000000, -6.500000000000000000 ) ) ;
#19343 = DIRECTION ( 'NONE',  ( -0.000000000000000000, -0.000000000000000000, 1.000000000000000000 ) ) ;
#19344 = VERTEX_POINT ( 'NONE', #2485 ) ;
#19345 = CARTESIAN_POINT ( 'NONE',  ( 3.756430356250004987, 29.75312499938549138, 8.999999999999992895 ) ) ;
#19346 = CARTESIAN_POINT ( 'NONE',  ( 0.000000000000000000, 0.000000000000000000, -6.500000000000000000 ) ) ;
#19348 = ORIENTED_EDGE ( 'NONE', *, *, #15056, .F. ) ;
#19347 = CARTESIAN_POINT ( 'NONE',  ( 0.000000000000000000, 0.000000000000000000, -6.500000000000000000 ) ) ;
#19349 = VECTOR ( 'NONE', #4097, 1000.000000000000000 ) ;
#19350 = ORIENTED_EDGE ( 'NONE', *, *, #9525, .F. ) ;
#19351 = ORIENTED_EDGE ( 'NONE', *, *, #19062, .T. ) ;
#19352 = VERTEX_POINT ( 'NONE', #2624 ) ;
#19353 = ORIENTED_EDGE ( 'NONE', *, *, #18813, .F. ) ;
#19354 = CARTESIAN_POINT ( 'NONE',  ( 29.72853858738278987, -9.133673601486577809, -2.750000000000000000 ) ) ;
#19355 = CYLINDRICAL_SURFACE ( 'NONE', #3170, 31.10000000000000142 ) ;
#19356 = CARTESIAN_POINT ( 'NONE',  ( 23.85222316637486273, 18.19536891688240843, 8.999999999999992895 ) ) ;
#19357 = MECHANICAL_DESIGN_GEOMETRIC_PRESENTATION_REPRESENTATION (  '', ( #12686 ), #22713 ) ;
#19358 = CARTESIAN_POINT ( 'NONE',  ( -1.878215178124995832, -5.746835883940462963, 2.540624999385482141 ) ) ;
#19359 = CARTESIAN_POINT ( 'NONE',  ( -3.999999999999996447, -8.999999999999992895, 1.068749998770966103 ) ) ;
#19360 = SURFACE_STYLE_FILL_AREA ( #17791 ) ;
#19361 = CARTESIAN_POINT ( 'NONE',  ( 3.756430356250002323, 28.81562499938548427, 11.16877607737301226 ) ) ;
#19362 = CIRCLE ( 'NONE', #8104, 31.10000000000000142 ) ;
#19363 = DIRECTION ( 'NONE',  ( 1.000000000000000000, 0.000000000000000000, 0.000000000000000000 ) ) ;
#19364 = LINE ( 'NONE', #19102, #18059 ) ;
#19365 = CARTESIAN_POINT ( 'NONE',  ( 2.000000000000000888, -12.46410161513774817, 1.274999999999998357 ) ) ;
#19366 = DIRECTION ( 'NONE',  ( 1.000000000000000000, 0.000000000000000000, 0.000000000000000000 ) ) ;
#19367 = DIRECTION ( 'NONE',  ( 1.000000000000000000, 0.000000000000000000, 0.000000000000000000 ) ) ;
#19368 = CARTESIAN_POINT ( 'NONE',  ( -5.706339097770933400, 38.63519838069944967, 7.645898033750358813 ) ) ;
#19369 = CARTESIAN_POINT ( 'NONE',  ( -4.000000000000003553, -25.88124999877096499, 6.690598923241489970 ) ) ;
#19370 = CARTESIAN_POINT ( 'NONE',  ( -3.756430356249996994, -8.999999999999992895, 4.078124999385482674 ) ) ;
#19371 = DIRECTION ( 'NONE',  ( -0.000000000000000000, -0.000000000000000000, 1.000000000000000000 ) ) ;
#19372 = CARTESIAN_POINT ( 'NONE',  ( 2.620986760973688460E-15, -13.61880215351699874, 4.781249998770964460 ) ) ;
#19373 = DIRECTION ( 'NONE',  ( 1.000000000000000000, 0.000000000000000000, 0.000000000000000000 ) ) ;
#19374 = ORIENTED_EDGE ( 'NONE', *, *, #3265, .T. ) ;
#19375 = EDGE_CURVE ( 'NONE', #15991, #23923, #6647, .T. ) ;
#19376 = DIRECTION ( 'NONE',  ( -0.000000000000000000, -1.000000000000000000, -0.000000000000000000 ) ) ;
#19377 = ORIENTED_EDGE ( 'NONE', *, *, #4807, .F. ) ;
#19378 = ORIENTED_EDGE ( 'NONE', *, *, #4692, .F. ) ;
#19379 = CARTESIAN_POINT ( 'NONE',  ( -3.526711513754773986, 29.50000000000000000, 13.85410196624972201 ) ) ;
#19380 = ORIENTED_EDGE ( 'NONE', *, *, #22619, .F. ) ;
#19381 = CARTESIAN_POINT ( 'NONE',  ( -3.735045420075836212E-15, -28.51562499938549067, 4.662447845253954171 ) ) ;
#19382 = VERTEX_POINT ( 'NONE', #12694 ) ;
#19383 = CARTESIAN_POINT ( 'NONE',  ( 4.000000000000003553, 26.80000000000000071, 8.999999999999992895 ) ) ;
#19384 = ADVANCED_FACE ( 'NONE', ( #6413 ), #14401, .T. ) ;
#19385 = EDGE_LOOP ( 'NONE', ( #5175, #11816, #1698, #24914 ) ) ;
#19386 = EDGE_CURVE ( 'NONE', #3288, #5826, #22490, .T. ) ;
#19387 = CARTESIAN_POINT ( 'NONE',  ( 2.000000000000000888, 28.07500000000000284, 12.46410161513774817 ) ) ;
#19388 = CARTESIAN_POINT ( 'NONE',  ( 4.000000000000002665, 29.46250000000000568, 11.30940107675849760 ) ) ;
#19389 = CARTESIAN_POINT ( 'NONE',  ( 4.000000000000001776, 26.31250000000000000, 11.30940107675849760 ) ) ;
#19390 = CARTESIAN_POINT ( 'NONE',  ( -1.071796769724489895, 25.76740381056767148, 12.99999999999999289 ) ) ;
#19391 = CARTESIAN_POINT ( 'NONE',  ( 18.17485398475098535, 18.17485398475091785, 4.662447845253954171 ) ) ;
#19392 = EDGE_CURVE ( 'NONE', #9972, #13686, #17004, .T. ) ;
#19393 = DIRECTION ( 'NONE',  ( -0.000000000000000000, -0.000000000000000000, -1.000000000000000000 ) ) ;
#19394 = ORIENTED_EDGE ( 'NONE', *, *, #707, .F. ) ;
#19395 = CARTESIAN_POINT ( 'NONE',  ( 4.000000000000003553, 26.80000000000000071, 8.999999999999992895 ) ) ;
#19396 = CIRCLE ( 'NONE', #18237, 8.000000000000000000 ) ;
#19397 = CARTESIAN_POINT ( 'NONE',  ( 21.04090992281141581, 18.38471254485196837, 12.25316411605952283 ) ) ;
#19398 = DIRECTION ( 'NONE',  ( 0.000000000000000000, -1.000000000000000000, 0.000000000000000000 ) ) ;
#19399 = ADVANCED_FACE ( 'NONE', ( #17273 ), #7316, .T. ) ;
#19400 = ORIENTED_EDGE ( 'NONE', *, *, #10621, .T. ) ;
#19401 = ORIENTED_EDGE ( 'NONE', *, *, #12668, .F. ) ;
#19402 = CARTESIAN_POINT ( 'NONE',  ( 4.000000000000002665, 28.50624999877097210, 11.30940107675849760 ) ) ;
#19403 = CARTESIAN_POINT ( 'NONE',  ( -3.756430356250003655, -29.19062499938548072, 8.999999999999992895 ) ) ;
#19404 = ORIENTED_EDGE ( 'NONE', *, *, #3597, .T. ) ;
#19405 = LINE ( 'NONE', #6866, #24213 ) ;
#19406 = CARTESIAN_POINT ( 'NONE',  ( 1.878215178125000939, 26.97812499938548569, 12.25316411605952283 ) ) ;
#19407 = CARTESIAN_POINT ( 'NONE',  ( 2.000000000000003997, 28.16874999877096997, 5.535898384862238508 ) ) ;
#19408 = VERTEX_POINT ( 'NONE', #13330 ) ;
#19409 = ORIENTED_EDGE ( 'NONE', *, *, #11449, .F. ) ;
#19410 = DIRECTION ( 'NONE',  ( 0.000000000000000000, 0.000000000000000000, 1.000000000000000000 ) ) ;
#19411 = ORIENTED_EDGE ( 'NONE', *, *, #6894, .F. ) ;
#19412 = CARTESIAN_POINT ( 'NONE',  ( -3.735045420075836212E-15, -28.06562499938548427, 4.662447845253954171 ) ) ;
#19413 = CARTESIAN_POINT ( 'NONE',  ( 3.756430356250004099, 25.62812499938548072, 6.831223922626973533 ) ) ;
#19414 = CARTESIAN_POINT ( 'NONE',  ( 3.756430356250000546, 29.15312499938548996, 11.16877607737301403 ) ) ;
#19415 = CARTESIAN_POINT ( 'NONE',  ( -19.32388608118395013, 23.96296185032730364, -6.500000000000000000 ) ) ;
#19416 = CARTESIAN_POINT ( 'NONE',  ( 6.009258394948636914E-15, 26.46250000000000213, 4.381197846482986158 ) ) ;
#19417 = ADVANCED_FACE ( 'NONE', ( #3386 ), #11104, .F. ) ;
#19418 = EDGE_CURVE ( 'NONE', #14884, #13396, #18622, .T. ) ;
#19419 = LINE ( 'NONE', #17349, #9584 ) ;
#19420 = EDGE_CURVE ( 'NONE', #24200, #7103, #12073, .T. ) ;
#19421 = DIRECTION ( 'NONE',  ( 1.000000000000000000, 0.000000000000000000, 0.000000000000000000 ) ) ;
#19422 = CARTESIAN_POINT ( 'NONE',  ( -3.756430356249996994, 26.26562499938548711, 8.999999999999992895 ) ) ;
#19423 = AXIS2_PLACEMENT_3D ( 'NONE', #6508, #4541, #14492 ) ;
#19424 = AXIS2_PLACEMENT_3D ( 'NONE', #12433, #16383, #6430 ) ;
#19425 = DIRECTION ( 'NONE',  ( -0.000000000000000000, 1.000000000000000000, -0.000000000000000000 ) ) ;
#19426 = CARTESIAN_POINT ( 'NONE',  ( 18.71181319714904845, 18.71181319714898095, 4.381197846482986158 ) ) ;
#19427 = CARTESIAN_POINT ( 'NONE',  ( 20.72271187127746828, 18.06651449331802439, 12.25316411605952283 ) ) ;
#19428 = CARTESIAN_POINT ( 'NONE',  ( -7.901901826148023498E-15, 28.71250000000000568, 4.999999999999992006 ) ) ;
#19429 = CARTESIAN_POINT ( 'NONE',  ( 1.878215178125000939, 29.56562499938548427, 12.25316411605952283 ) ) ;
#19430 = CARTESIAN_POINT ( 'NONE',  ( -30.04913349766215802, 5.827558883616378083, -6.500000000000000000 ) ) ;
#19431 = EDGE_CURVE ( 'NONE', #16617, #19775, #11363, .T. ) ;
#19432 = CARTESIAN_POINT ( 'NONE',  ( 16.26111872703749128, 21.57351348295617299, 11.16877607737301048 ) ) ;
#19433 = CARTESIAN_POINT ( 'NONE',  ( 30.24338421796779386, -7.248980000274303670, -6.500000000000000000 ) ) ;
#19434 = ORIENTED_EDGE ( 'NONE', *, *, #4168, .T. ) ;
#19435 = CARTESIAN_POINT ( 'NONE',  ( 3.999999999999997335, -25.71250000000000213, 11.30940107675849404 ) ) ;
#19437 = ORIENTED_EDGE ( 'NONE', *, *, #21059, .F. ) ;
#19436 = DIRECTION ( 'NONE',  ( 0.000000000000000000, -0.000000000000000000, 1.000000000000000000 ) ) ;
#19438 = CARTESIAN_POINT ( 'NONE',  ( 1.878215178125004048, 25.77812499938548640, 5.746835883940462963 ) ) ;
#19439 = CARTESIAN_POINT ( 'NONE',  ( -0.7500000000000001110, 0.000000000000000000, 18.19999999999999929 ) ) ;
#19440 = CARTESIAN_POINT ( 'NONE',  ( 3.756430356249996994, -28.96562499938548285, 8.999999999999992895 ) ) ;
#19441 = EDGE_LOOP ( 'NONE', ( #5176, #16377, #9822, #5516 ) ) ;
#19442 = VERTEX_POINT ( 'NONE', #1437 ) ;
#19443 = CARTESIAN_POINT ( 'NONE',  ( 21.02609847369771501, 21.40030839749514868, 4.999999999999992895 ) ) ;
#19444 = CARTESIAN_POINT ( 'NONE',  ( 3.756430356250004543, 29.71562499938548996, 11.16877607737301226 ) ) ;
#19445 = EDGE_CURVE ( 'NONE', #132, #12485, #16250, .T. ) ;
#19446 = APPLICATION_CONTEXT ( 'automotive_design' ) ;
#19447 = CARTESIAN_POINT ( 'NONE',  ( 1.878215178125000939, -12.25316411605952283, 1.415624999385481253 ) ) ;
#19448 =( BOUNDED_CURVE ( )  B_SPLINE_CURVE ( 2, ( #6872, #22828, #6353, #4509, #14346, #22308, #20733, #22707, #20460 ),
 .UNSPECIFIED., .F., .F. ) 
 B_SPLINE_CURVE_WITH_KNOTS ( ( 3, 2, 2, 2, 3 ),
 ( 0.7249999999999999778, 0.7333333333333332815, 0.7500000000000000000, 0.7666666666666667185, 0.7750000000000000222 ),
 .UNSPECIFIED. ) 
 CURVE ( )  GEOMETRIC_REPRESENTATION_ITEM ( )  RATIONAL_B_SPLINE_CURVE ( ( 0.9330127018922194093, 0.9330127018922194093, 1.000000000000000000, 0.8660254037844387076, 1.000000000000000000, 0.8660254037844387076, 1.000000000000000000, 0.9330127018922194093, 0.9330127018922194093 ) ) 
 REPRESENTATION_ITEM ( '' )  );
#19449 = EDGE_CURVE ( 'NONE', #9415, #10376, #11492, .T. ) ;
#19450 = B_SPLINE_CURVE_WITH_KNOTS ( 'NONE', 3,
 ( #23665, #5240, #15310, #13220, #21189, #1708, #15575, #19356 ),
 .UNSPECIFIED., .F., .F.,
 ( 4, 2, 2, 4 ),
 ( 0.01599790909976502723, 0.01669365098321972177, 0.01738939286667441977, 0.01878087663358380885 ),
 .UNSPECIFIED. ) ;
#19451 = CARTESIAN_POINT ( 'NONE',  ( -3.756430356249996994, -8.999999999999992895, 3.628124999385483829 ) ) ;
#19452 = CARTESIAN_POINT ( 'NONE',  ( 27.09999999999999787, 0.6000000000000000888, 19.59999999999999787 ) ) ;
#19453 =( BOUNDED_CURVE ( )  B_SPLINE_CURVE ( 2, ( #4803, #20622, #16574, #24930, #16963, #1009, #12650, #13040, #21019 ),
 .UNSPECIFIED., .F., .F. ) 
 B_SPLINE_CURVE_WITH_KNOTS ( ( 3, 2, 2, 2, 3 ),
 ( 0.2750000000000000222, 0.2833333333333333259, 0.2999999999999999889, 0.3166666666666666519, 0.3250000000000000111 ),
 .UNSPECIFIED. ) 
 CURVE ( )  GEOMETRIC_REPRESENTATION_ITEM ( )  RATIONAL_B_SPLINE_CURVE ( ( 0.9330127018922194093, 0.9330127018922196314, 1.000000000000000000, 0.8660254037844387076, 1.000000000000000000, 0.8660254037844387076, 1.000000000000000000, 0.9330127018922191873, 0.9330127018922194093 ) ) 
 REPRESENTATION_ITEM ( '' )  );
#19454 = CARTESIAN_POINT ( 'NONE',  ( 28.72825533807124287, -11.91206721063061913, -2.750000000000000000 ) ) ;
#19455 = CARTESIAN_POINT ( 'NONE',  ( -31.00322564728512020, 2.451530025009346581, 1.000000000000000000 ) ) ;
#19456 = PLANE ( 'NONE',  #1995 ) ;
#19457 = CARTESIAN_POINT ( 'NONE',  ( -3.137519842735244810E-15, 26.85624999877096641, 4.999999999999991118 ) ) ;
#19458 = FACE_OUTER_BOUND ( 'NONE', #306, .T. ) ;
#19459 = ORIENTED_EDGE ( 'NONE', *, *, #13607, .F. ) ;
#19460 = CARTESIAN_POINT ( 'NONE',  ( -2.000000000000000888, -29.81874999877096855, 12.46410161513774817 ) ) ;
#19461 = LINE ( 'NONE', #1553, #63 ) ;
#19462 = CARTESIAN_POINT ( 'NONE',  ( -3.756430356249996994, 28.62812499938548427, 8.999999999999992895 ) ) ;
#19464 = EDGE_CURVE ( 'NONE', #22072, #14822, #15117, .T. ) ;
#19463 = DIRECTION ( 'NONE',  ( 1.000000000000000000, 0.000000000000000000, 0.000000000000000000 ) ) ;
#19465 = CARTESIAN_POINT ( 'NONE',  ( 1.071796769724494558, 27.34240381056766722, 4.999999999999992895 ) ) ;
#19466 = DIRECTION ( 'NONE',  ( 0.000000000000000000, 0.000000000000000000, 1.000000000000000000 ) ) ;
#19467 = VERTEX_POINT ( 'NONE', #21058 ) ;
#19468 = CARTESIAN_POINT ( 'NONE',  ( 19.43607991388971712, -24.27856662945514543, -6.500000000000000000 ) ) ;
#19470 = ORIENTED_EDGE ( 'NONE', *, *, #21818, .F. ) ;
#19469 = CARTESIAN_POINT ( 'NONE',  ( -1.071796769724495668, -26.25759618943233065, 12.99999999999999112 ) ) ;
#19471 = EDGE_LOOP ( 'NONE', ( #9708, #7855, #3198, #13342 ) ) ;
#19472 = ORIENTED_EDGE ( 'NONE', *, *, #18335, .T. ) ;
#19473 = ORIENTED_EDGE ( 'NONE', *, *, #20905, .T. ) ;
#19474 = EDGE_LOOP ( 'NONE', ( #14555, #18940, #23299, #14411 ) ) ;
#19475 = DIRECTION ( 'NONE',  ( 0.000000000000000000, 0.000000000000000000, -1.000000000000000000 ) ) ;
#19476 = CARTESIAN_POINT ( 'NONE',  ( 0.000000000000000000, 0.000000000000000000, -6.500000000000000000 ) ) ;
#19477 = CARTESIAN_POINT ( 'NONE',  ( 3.756430356250002323, 25.62812499938548072, 6.831223922626973533 ) ) ;
#19478 = CARTESIAN_POINT ( 'NONE',  ( -3.756430356249995661, -6.831223922626973533, 3.028124999385485072 ) ) ;
#19479 = CARTESIAN_POINT ( 'NONE',  ( -3.999999999999997335, -11.30940107675849404, 2.906249998770968457 ) ) ;
#19480 = CARTESIAN_POINT ( 'NONE',  ( -3.756430356249996994, 28.62812499938548427, 8.999999999999992895 ) ) ;
#19481 = DIRECTION ( 'NONE',  ( 0.000000000000000000, 0.000000000000000000, 1.000000000000000000 ) ) ;
#19482 = DIRECTION ( 'NONE',  ( -0.000000000000000000, -0.000000000000000000, -1.000000000000000000 ) ) ;
#19484 = EDGE_CURVE ( 'NONE', #822, #13339, #22519, .T. ) ;
#19483 = CARTESIAN_POINT ( 'NONE',  ( 2.000000000000003997, -5.535898384862238508, 1.424999999999999156 ) ) ;
#19485 = DIRECTION ( 'NONE',  ( 0.000000000000000000, 0.000000000000000000, -1.000000000000000000 ) ) ;
#19486 = CARTESIAN_POINT ( 'NONE',  ( -3.999999999999996447, -8.999999999999992895, 18.00000000000000000 ) ) ;
#19487 = CARTESIAN_POINT ( 'NONE',  ( 28.91604871112465602, 11.44867358849340633, -6.500000000000000000 ) ) ;
#19488 = CARTESIAN_POINT ( 'NONE',  ( 1.999999999999998224, -26.59374999877096712, 12.46410161513774639 ) ) ;
#19489 = CARTESIAN_POINT ( 'NONE',  ( 1.878215178125000939, 29.22812499938548569, 12.25316411605952283 ) ) ;
#19490 = CARTESIAN_POINT ( 'NONE',  ( -7.248980000274416469, -30.24338421796776544, -2.750000000000000000 ) ) ;
#19491 = DIRECTION ( 'NONE',  ( -1.000000000000000000, 0.000000000000000000, 0.000000000000000000 ) ) ;
#19492 = CARTESIAN_POINT ( 'NONE',  ( 3.834746474454188013E-15, 28.20624999877096428, 4.999999999999992006 ) ) ;
#19493 = ORIENTED_EDGE ( 'NONE', *, *, #22944, .T. ) ;
#19494 = PLANE ( 'NONE',  #3730 ) ;
#19495 = EDGE_LOOP ( 'NONE', ( #6428, #11201, #20388, #23032 ) ) ;
#19496 = VERTEX_POINT ( 'NONE', #17508 ) ;
#19497 = FACE_OUTER_BOUND ( 'NONE', #16400, .T. ) ;
#19498 = ORIENTED_EDGE ( 'NONE', *, *, #10685, .F. ) ;
#19499 = CARTESIAN_POINT ( 'NONE',  ( -3.756430356250004099, -28.89062499938548356, 6.831223922626973533 ) ) ;
#19500 = ORIENTED_EDGE ( 'NONE', *, *, #6669, .F. ) ;
#19501 = CARTESIAN_POINT ( 'NONE',  ( 3.469446951953614189E-15, 35.50000000000000711, 8.999999999999992895 ) ) ;
#19502 = ORIENTED_EDGE ( 'NONE', *, *, #2772, .F. ) ;
#19503 = CARTESIAN_POINT ( 'NONE',  ( 2.620986760973688460E-15, 27.13750000000000284, 13.61880215351699874 ) ) ;
#19504 = CARTESIAN_POINT ( 'NONE',  ( -31.09598070739550124, 0.4999838450263022760, -6.500000000000000000 ) ) ;
#19505 = CARTESIAN_POINT ( 'NONE',  ( -1.878215178124995832, -5.746835883940462963, 1.303124999385483429 ) ) ;
#19506 = CARTESIAN_POINT ( 'NONE',  ( 0.000000000000000000, 0.000000000000000000, -6.500000000000000000 ) ) ;
#19507 = CARTESIAN_POINT ( 'NONE',  ( 23.40315227927642283, 18.09075752335759901, 6.831223922626973533 ) ) ;
#19508 = DIRECTION ( 'NONE',  ( 0.000000000000000000, 0.000000000000000000, -1.000000000000000000 ) ) ;
#19509 = EDGE_CURVE ( 'NONE', #19338, #11048, #25116, .T. ) ;
#19510 = CARTESIAN_POINT ( 'NONE',  ( 4.000000000000001776, 28.11250000000000426, 11.30940107675849760 ) ) ;
#19511 = EDGE_CURVE ( 'NONE', #6676, #12074, #21176, .T. ) ;
#19512 = CARTESIAN_POINT ( 'NONE',  ( 4.000000000000003553, 25.93750000000000000, 6.690598923241489970 ) ) ;
#19513 = CARTESIAN_POINT ( 'NONE',  ( -4.000000000000003553, -29.44374999877096855, 8.999999999999992895 ) ) ;
#19514 = VERTEX_POINT ( 'NONE', #3770 ) ;
#19516 = EDGE_CURVE ( 'NONE', #23656, #8280, #7894, .T. ) ;
#19515 = ORIENTED_EDGE ( 'NONE', *, *, #4168, .F. ) ;
#19517 = CARTESIAN_POINT ( 'NONE',  ( 4.000000000000003553, 27.64374999877097139, 8.999999999999992895 ) ) ;
#19518 = VERTEX_POINT ( 'NONE', #2211 ) ;
#19519 = CARTESIAN_POINT ( 'NONE',  ( 1.071796769724491227, 26.44240381056766509, 4.999999999999989342 ) ) ;
#19520 = CARTESIAN_POINT ( 'NONE',  ( 1.878215178125004048, 28.02812499938548640, 5.746835883940462963 ) ) ;
#19521 = CYLINDRICAL_SURFACE ( 'NONE', #22148, 31.10000000000000142 ) ;
#19522 = EDGE_CURVE ( 'NONE', #23624, #12737, #25851, .T. ) ;
#19523 = VERTEX_POINT ( 'NONE', #15803 ) ;
#19524 = EDGE_LOOP ( 'NONE', ( #934, #2500 ) ) ;
#19525 = AXIS2_PLACEMENT_3D ( 'NONE', #15457, #9939, #13743 ) ;
#19526 = DIRECTION ( 'NONE',  ( 0.000000000000000000, 0.000000000000000000, 1.000000000000000000 ) ) ;
#19527 = ORIENTED_EDGE ( 'NONE', *, *, #9750, .T. ) ;
#19528 = CARTESIAN_POINT ( 'NONE',  ( 3.434593913234900153, 38.94978637201472793, 4.639884373247868510 ) ) ;
#19529 = LINE ( 'NONE', #11830, #15973 ) ;
#19530 = CARTESIAN_POINT ( 'NONE',  ( -1.878215178124994722, 27.99062499938548143, 5.746835883940462963 ) ) ;
#19531 = VECTOR ( 'NONE', #3357, 1000.000000000000000 ) ;
#19532 = DIRECTION ( 'NONE',  ( 0.000000000000000000, 0.000000000000000000, 1.000000000000000000 ) ) ;
#19533 = CARTESIAN_POINT ( 'NONE',  ( -3.999999999999996447, 26.08750000000000213, 6.690598923241487306 ) ) ;
#19534 = CARTESIAN_POINT ( 'NONE',  ( 2.672651547586948120E-15, 27.72812499938548569, 13.33755215474602984 ) ) ;
#19535 = DIRECTION ( 'NONE',  ( 0.000000000000000000, 0.000000000000000000, 1.000000000000000000 ) ) ;
#19536 = DIRECTION ( 'NONE',  ( -0.000000000000000000, -1.000000000000000000, -0.000000000000000000 ) ) ;
#19537 = EDGE_CURVE ( 'NONE', #17035, #23841, #18038, .T. ) ;
#19538 = CIRCLE ( 'NONE', #19565, 31.10000000000000142 ) ;
#19539 = CARTESIAN_POINT ( 'NONE',  ( 3.735045420075836212E-15, 28.85312499938548569, 4.662447845253954171 ) ) ;
#19540 = DIRECTION ( 'NONE',  ( 0.5358267949790093132, 0.8443279255020070817, 0.000000000000000000 ) ) ;
#19541 = CARTESIAN_POINT ( 'NONE',  ( 22.70696651085303941, 17.05011226136058866, 11.30940107675849760 ) ) ;
#19542 = CARTESIAN_POINT ( 'NONE',  ( 18.33167953626305646, 20.98787691422236179, 12.25316411605951927 ) ) ;
#19543 = DIRECTION ( 'NONE',  ( 0.000000000000000000, 1.000000000000000000, 0.000000000000000000 ) ) ;
#19544 = DIRECTION ( 'NONE',  ( 1.000000000000000000, 0.000000000000000000, 0.000000000000000000 ) ) ;
#19546 = DIRECTION ( 'NONE',  ( 0.4257792915650712717, -0.9048270524660203540, 0.000000000000000000 ) ) ;
#19545 = VECTOR ( 'NONE', #310, 1000.000000000000000 ) ;
#19547 = CARTESIAN_POINT ( 'NONE',  ( -22.67092431280609688, -21.28941499438201745, -6.500000000000000000 ) ) ;
#19548 = CARTESIAN_POINT ( 'NONE',  ( 4.000000000000005329, 25.88124999877097565, 6.690598923241489970 ) ) ;
#19549 = AXIS2_PLACEMENT_3D ( 'NONE', #12024, #13882, #2242 ) ;
#19550 = ORIENTED_EDGE ( 'NONE', *, *, #23567, .T. ) ;
#19551 = CARTESIAN_POINT ( 'NONE',  ( -3.999999999999996003, 26.03124999877097068, 6.690598923241487306 ) ) ;
#19552 = CARTESIAN_POINT ( 'NONE',  ( -4.000000000000001776, -27.21250000000000213, 11.30940107675849760 ) ) ;
#19553 = EDGE_CURVE ( 'NONE', #12264, #4065, #3302, .T. ) ;
#19555 = ORIENTED_EDGE ( 'NONE', *, *, #9570, .T. ) ;
#19554 = CARTESIAN_POINT ( 'NONE',  ( 4.006172263299091013E-15, 25.36562499938549564, 4.662447845253954171 ) ) ;
#19556 = CARTESIAN_POINT ( 'NONE',  ( -1.878215178124998497, 25.55312499938548854, 12.25316411605951927 ) ) ;
#19557 = EDGE_CURVE ( 'NONE', #8387, #18460, #18167, .T. ) ;
#19558 = CARTESIAN_POINT ( 'NONE',  ( 3.469446951953614189E-15, 30.00000000000000355, 4.999999999999992006 ) ) ;
#19559 = CARTESIAN_POINT ( 'NONE',  ( 25.98730014090442353, 17.08421000182768523, 1.000000000000000000 ) ) ;
#19560 = CARTESIAN_POINT ( 'NONE',  ( -26.25859848311247902, 16.66421332384710752, -6.500000000000000000 ) ) ;
#19561 = ORIENTED_EDGE ( 'NONE', *, *, #21132, .T. ) ;
#19562 = EDGE_LOOP ( 'NONE', ( #3116, #17620, #22645, #14020, #2490 ) ) ;
#19563 = DIRECTION ( 'NONE',  ( 0.000000000000000000, 0.000000000000000000, -1.000000000000000000 ) ) ;
#19564 = CARTESIAN_POINT ( 'NONE',  ( -3.756430356250000546, 29.56562499938549493, 11.16877607737301226 ) ) ;
#19565 = AXIS2_PLACEMENT_3D ( 'NONE', #2240, #8514, #6411 ) ;
#19566 = AXIS2_PLACEMENT_3D ( 'NONE', #19575, #25344, #23641 ) ;
#19567 = CARTESIAN_POINT ( 'NONE',  ( -1.878215178124998497, -12.25316411605951927, 0.8906249993854836733 ) ) ;
#19568 = CIRCLE ( 'NONE', #1217, 0.7500000000000001110 ) ;
#19569 = VECTOR ( 'NONE', #24035, 1000.000000000000000 ) ;
#19570 = DIRECTION ( 'NONE',  ( 0.000000000000000000, 0.000000000000000000, 1.000000000000000000 ) ) ;
#19571 = FILL_AREA_STYLE_COLOUR ( '', #16464 ) ;
#19572 = CARTESIAN_POINT ( 'NONE',  ( -1.071796769724494558, -27.34240381056766722, 4.999999999999992895 ) ) ;
#19573 = DIRECTION ( 'NONE',  ( -0.000000000000000000, -0.000000000000000000, -1.000000000000000000 ) ) ;
#19574 = DIRECTION ( 'NONE',  ( 0.000000000000000000, 0.000000000000000000, 1.000000000000000000 ) ) ;
#19575 = CARTESIAN_POINT ( 'NONE',  ( 0.000000000000000000, 0.000000000000000000, -6.500000000000000000 ) ) ;
#19576 = CARTESIAN_POINT ( 'NONE',  ( 4.000000000000003553, 25.84374999877096712, 8.999999999999992895 ) ) ;
#19577 = CARTESIAN_POINT ( 'NONE',  ( 15.25349156384666216, 20.56588631976534387, 6.831223922626973533 ) ) ;
#19578 = CARTESIAN_POINT ( 'NONE',  ( 21.76563060752939549, 16.10877635803694119, 6.690598923241489970 ) ) ;
#19579 = ORIENTED_EDGE ( 'NONE', *, *, #3890, .F. ) ;
#19580 = CARTESIAN_POINT ( 'NONE',  ( -28.14012133169333651, -13.24173596767349359, -6.500000000000000000 ) ) ;
#19581 = CARTESIAN_POINT ( 'NONE',  ( 4.000000000000002665, 29.73213749463701205, 8.735714247490120599 ) ) ;
#19582 = CARTESIAN_POINT ( 'NONE',  ( 1.878215178125000939, 28.77812499938548640, 12.25316411605952283 ) ) ;
#19583 = CYLINDRICAL_SURFACE ( 'NONE', #21639, 1.500000000000000222 ) ;
#19584 = AXIS2_PLACEMENT_3D ( 'NONE', #6152, #4192, #20390 ) ;
#19585 = CARTESIAN_POINT ( 'NONE',  ( -4.000000000000003553, -25.39374999877096784, 8.999999999999992895 ) ) ;
#19586 = EDGE_CURVE ( 'NONE', #12207, #4893, #17933, .T. ) ;
#19587 = ORIENTED_EDGE ( 'NONE', *, *, #12188, .F. ) ;
#19588 = CARTESIAN_POINT ( 'NONE',  ( -1.859271017917182139E-15, -27.08124999877096784, 12.99999999999999289 ) ) ;
#19589 = DIRECTION ( 'NONE',  ( 0.000000000000000000, 0.000000000000000000, 1.000000000000000000 ) ) ;
#19591 = ORIENTED_EDGE ( 'NONE', *, *, #20926, .T. ) ;
#19590 = CARTESIAN_POINT ( 'NONE',  ( 1.071796769724497222, 28.45134618820330275, 12.99999999999998757 ) ) ;
#19593 = EDGE_CURVE ( 'NONE', #17035, #18497, #1899, .T. ) ;
#19592 = AXIS2_PLACEMENT_3D ( 'NONE', #20283, #18331, #21996 ) ;
#19594 = VERTEX_POINT ( 'NONE', #23773 ) ;
#19595 = EDGE_LOOP ( 'NONE', ( #25216, #18731, #14620, #1566 ) ) ;
#19596 = ORIENTED_EDGE ( 'NONE', *, *, #13707, .F. ) ;
#19597 = ORIENTED_EDGE ( 'NONE', *, *, #9649, .T. ) ;
#19598 = DIRECTION ( 'NONE',  ( 0.7289686274214236539, 0.6845471059286760696, 0.000000000000000000 ) ) ;
#19599 =( BOUNDED_CURVE ( )  B_SPLINE_CURVE ( 2, ( #17677, #23674, #5751, #13738, #21715, #3799, #11 ),
 .UNSPECIFIED., .F., .F. ) 
 B_SPLINE_CURVE_WITH_KNOTS ( ( 3, 2, 2, 3 ),
 ( 0.4499999999999998446, 0.4666666666666665075, 0.4833333333333331150, 0.4999999999999997780 ),
 .UNSPECIFIED. ) 
 CURVE ( )  GEOMETRIC_REPRESENTATION_ITEM ( )  RATIONAL_B_SPLINE_CURVE ( ( 1.000000000000001332, 0.8660254037844373753, 1.000000000000000000, 0.8660254037844387076, 1.000000000000000000, 0.8660254037844404840, 0.9999999999999982236 ) ) 
 REPRESENTATION_ITEM ( '' )  );
#19600 = CARTESIAN_POINT ( 'NONE',  ( -20.78941499438192508, 22.67092431280617859, -6.500000000000000000 ) ) ;
#19601 = CIRCLE ( 'NONE', #2492, 31.10000000000000142 ) ;
#19602 = FACE_OUTER_BOUND ( 'NONE', #24615, .T. ) ;
#19603 = CYLINDRICAL_SURFACE ( 'NONE', #8905, 0.5000000000000004441 ) ;
#19604 =( BOUNDED_CURVE ( )  B_SPLINE_CURVE ( 2, ( #9494, #9382, #23621, #25072, #15655, #15529, #11329, #9252, #17609 ),
 .UNSPECIFIED., .F., .F. ) 
 B_SPLINE_CURVE_WITH_KNOTS ( ( 3, 2, 2, 2, 3 ),
 ( 0.2750000000000000222, 0.2833333333333333259, 0.2999999999999999889, 0.3166666666666666519, 0.3250000000000000111 ),
 .UNSPECIFIED. ) 
 CURVE ( )  GEOMETRIC_REPRESENTATION_ITEM ( )  RATIONAL_B_SPLINE_CURVE ( ( 0.9330127018922194093, 0.9330127018922196314, 1.000000000000000000, 0.8660254037844387076, 1.000000000000000000, 0.8660254037844387076, 1.000000000000000000, 0.9330127018922191873, 0.9330127018922194093 ) ) 
 REPRESENTATION_ITEM ( '' )  );
#19605 = AXIS2_PLACEMENT_3D ( 'NONE', #16453, #1006, #16959 ) ;
#19606 = CIRCLE ( 'NONE', #1226, 0.4999999999999996669 ) ;
#19607 = CARTESIAN_POINT ( 'NONE',  ( -1.878215178124998497, -12.25316411605951927, 2.240624999385484095 ) ) ;
#19608 = CARTESIAN_POINT ( 'NONE',  ( 4.000000000000001776, -11.30940107675849760, 1.706249998770968945 ) ) ;
#19609 = CARTESIAN_POINT ( 'NONE',  ( -3.756430356249995661, 29.04062499938548569, 6.831223922626973533 ) ) ;
#19610 = VECTOR ( 'NONE', #8324, 999.9999999999998863 ) ;
#19611 = CARTESIAN_POINT ( 'NONE',  ( 0.5000000000000000000, 0.000000000000000000, 19.50000000000000000 ) ) ;
#19612 = CARTESIAN_POINT ( 'NONE',  ( 4.000000000000003553, 28.54374999877096997, 8.999999999999992895 ) ) ;
#19613 = CARTESIAN_POINT ( 'NONE',  ( -3.999999999999997335, -11.30940107675849404, 2.962499999999996803 ) ) ;
#19614 = DIRECTION ( 'NONE',  ( 0.000000000000000000, 1.000000000000000000, 0.000000000000000000 ) ) ;
#19615 = DIRECTION ( 'NONE',  ( -0.000000000000000000, -0.000000000000000000, 1.000000000000000000 ) ) ;
#19616 = FACE_OUTER_BOUND ( 'NONE', #3322, .T. ) ;
#19617 = CARTESIAN_POINT ( 'NONE',  ( -2.000000000000000888, -27.56874999877096855, 12.46410161513774817 ) ) ;
#19618 = CARTESIAN_POINT ( 'NONE',  ( -3.756430356249997882, 28.66562499938548569, 11.16877607737301226 ) ) ;
#19619 = CARTESIAN_POINT ( 'NONE',  ( -26.25859848311282363, -16.66421332384654974, -6.500000000000000000 ) ) ;
#19620 = VECTOR ( 'NONE', #10258, 1000.000000000000000 ) ;
#19621 = CYLINDRICAL_SURFACE ( 'NONE', #792, 4.000000000000000000 ) ;
#19622 = FACE_OUTER_BOUND ( 'NONE', #13008, .T. ) ;
#19623 = ORIENTED_EDGE ( 'NONE', *, *, #25197, .F. ) ;
#19624 = CARTESIAN_POINT ( 'NONE',  ( -9.296355089585910693E-16, 26.91250000000000497, 4.999999999999991118 ) ) ;
#19625 = VERTEX_POINT ( 'NONE', #9790 ) ;
#19626 = EDGE_CURVE ( 'NONE', #13647, #14723, #22098, .T. ) ;
#19627 = AXIS2_PLACEMENT_3D ( 'NONE', #10804, #4927, #24937 ) ;
#19628 = VERTEX_POINT ( 'NONE', #19585 ) ;
#19629 = LINE ( 'NONE', #13628, #21712 ) ;
#19630 = VERTEX_POINT ( 'NONE', #11877 ) ;
#19631 = CARTESIAN_POINT ( 'NONE',  ( -3.735045420075836212E-15, -27.61562499938548498, 4.662447845253954171 ) ) ;
#19632 = VERTEX_POINT ( 'NONE', #24157 ) ;
#19633 = CYLINDRICAL_SURFACE ( 'NONE', #518, 4.000000000000000000 ) ;
#19634 = CIRCLE ( 'NONE', #24660, 31.10000000000000142 ) ;
#19635 = ADVANCED_FACE ( 'NONE', ( #17769 ), #6248, .F. ) ;
#19636 = VERTEX_POINT ( 'NONE', #9908 ) ;
#19637 = CARTESIAN_POINT ( 'NONE',  ( 2.620986760973688460E-15, 26.68750000000000000, 13.61880215351699874 ) ) ;
#19638 = CARTESIAN_POINT ( 'NONE',  ( 0.000000000000000000, 0.000000000000000000, -6.500000000000000000 ) ) ;
#19639 = EDGE_CURVE ( 'NONE', #8528, #16342, #22286, .T. ) ;
#19640 = AXIS2_PLACEMENT_3D ( 'NONE', #23595, #23710, #3460 ) ;
#19641 = DIRECTION ( 'NONE',  ( 0.000000000000000000, 0.000000000000000000, 1.000000000000000000 ) ) ;
#19642 = DIRECTION ( 'NONE',  ( 0.000000000000000000, 0.000000000000000000, -1.000000000000000000 ) ) ;
#19643 = CARTESIAN_POINT ( 'NONE',  ( 16.55507374853184999, 19.21127112649115531, 5.746835883940462963 ) ) ;
#19644 = AXIS2_PLACEMENT_3D ( 'NONE', #14904, #11215, #9276 ) ;
#19645 = CARTESIAN_POINT ( 'NONE',  ( -4.000000000000000000, 27.41874999877096997, 8.999999999999992895 ) ) ;
#19646 = AXIS2_PLACEMENT_3D ( 'NONE', #16738, #24707, #14643 ) ;
#19647 = FACE_OUTER_BOUND ( 'NONE', #6005, .T. ) ;
#19648 = CARTESIAN_POINT ( 'NONE',  ( 2.620986760973688460E-15, 28.03750000000000142, 13.61880215351699874 ) ) ;
#19649 = CIRCLE ( 'NONE', #8389, 0.5000000000000007772 ) ;
#19650 = CARTESIAN_POINT ( 'NONE',  ( 1.859271017917182139E-15, 29.38749999999999929, 12.99999999999999289 ) ) ;
#19651 = CARTESIAN_POINT ( 'NONE',  ( 18.24985654912466515, 23.56225130504333620, 11.16877607737301048 ) ) ;
#19652 = DIRECTION ( 'NONE',  ( 0.000000000000000000, 0.000000000000000000, 1.000000000000000000 ) ) ;
#19653 = EDGE_LOOP ( 'NONE', ( #25337, #6861, #2814, #3358 ) ) ;
#19654 = EDGE_LOOP ( 'NONE', ( #25210, #12332, #10381, #20209 ) ) ;
#19655 = CARTESIAN_POINT ( 'NONE',  ( 3.756430356250004543, 25.29062499938548925, 6.831223922626973533 ) ) ;
#19656 = ORIENTED_EDGE ( 'NONE', *, *, #15128, .T. ) ;
#19657 = CYLINDRICAL_SURFACE ( 'NONE', #17950, 0.5000000000000004441 ) ;
#19658 = VECTOR ( 'NONE', #165, 1000.000000000000000 ) ;
#19659 = CARTESIAN_POINT ( 'NONE',  ( 3.735045420075836212E-15, 29.41562499938548569, 4.662447845253954171 ) ) ;
#19660 = CARTESIAN_POINT ( 'NONE',  ( 3.834746474454188013E-15, 28.20624999877096428, 4.999999999999992006 ) ) ;
#19661 = ORIENTED_EDGE ( 'NONE', *, *, #17300, .F. ) ;
#19662 = ORIENTED_EDGE ( 'NONE', *, *, #3860, .F. ) ;
#19663 = AXIS2_PLACEMENT_3D ( 'NONE', #12654, #24537, #2709 ) ;
#19664 = VECTOR ( 'NONE', #656, 1000.000000000000000 ) ;
#19665 = ADVANCED_FACE ( 'NONE', ( #11992 ), #22598, .T. ) ;
#19666 = DIRECTION ( 'NONE',  ( 0.000000000000000000, 0.000000000000000000, -1.000000000000000000 ) ) ;
#19667 = VERTEX_POINT ( 'NONE', #16709 ) ;
#19668 = DIRECTION ( 'NONE',  ( -1.000000000000000000, 0.000000000000000000, 0.000000000000000000 ) ) ;
#19669 = CARTESIAN_POINT ( 'NONE',  ( 3.756430356250004099, 25.17812499938548498, 6.831223922626973533 ) ) ;
#19670 = CARTESIAN_POINT ( 'NONE',  ( 3.756430356250004099, 27.87812499938548783, 6.831223922626973533 ) ) ;
#19671 = AXIS2_PLACEMENT_3D ( 'NONE', #7519, #19536, #17085 ) ;
#19672 = EDGE_CURVE ( 'NONE', #11524, #2254, #8479, .T. ) ;
#19673 = EDGE_CURVE ( 'NONE', #20210, #1627, #24426, .T. ) ;
#19674 = CARTESIAN_POINT ( 'NONE',  ( -1.071796769724491227, -26.89240381056766793, 4.999999999999989342 ) ) ;
#19675 = CARTESIAN_POINT ( 'NONE',  ( -3.999999999999994671, 26.98750000000000782, 6.690598923241487306 ) ) ;
#19676 = CIRCLE ( 'NONE', #19254, 0.5000000000000006661 ) ;
#19677 = EDGE_CURVE ( 'NONE', #19667, #11616, #1626, .T. ) ;
#19678 = CARTESIAN_POINT ( 'NONE',  ( 29.41953157733086854, -10.08469938919509623, -6.500000000000000000 ) ) ;
#19679 = SURFACE_SIDE_STYLE ('',( #4467 ) ) ;
#19680 = VECTOR ( 'NONE', #10556, 1000.000000000000000 ) ;
#19681 = VECTOR ( 'NONE', #18026, 1000.000000000000000 ) ;
#19682 = DIRECTION ( 'NONE',  ( -0.9921147013144785420, -0.1253332335642980688, 0.000000000000000000 ) ) ;
#19683 = DIRECTION ( 'NONE',  ( -0.6845471059286831750, 0.7289686274214168815, 0.000000000000000000 ) ) ;
#19684 = CARTESIAN_POINT ( 'NONE',  ( 18.27871029367229383, 21.10713741841841085, 5.535898384862237620 ) ) ;
#19685 = CARTESIAN_POINT ( 'NONE',  ( 23.37663577498192780, 18.06424101906310753, 8.999999999999992895 ) ) ;
#19686 = CARTESIAN_POINT ( 'NONE',  ( -3.347751660414011177, -29.81285215011482137, 11.20140010723572388 ) ) ;
#19687 = DIRECTION ( 'NONE',  ( 0.000000000000000000, -0.000000000000000000, -1.000000000000000000 ) ) ;
#19688 = CIRCLE ( 'NONE', #25136, 0.5000000000000007772 ) ;
#19689 = CARTESIAN_POINT ( 'NONE',  ( 2.000000000000003553, 27.26874999877097494, 5.535898384862238508 ) ) ;
#19690 = FACE_BOUND ( 'NONE', #23682, .T. ) ;
#19691 = CYLINDRICAL_SURFACE ( 'NONE', #18817, 4.000000000000000000 ) ;
#19692 = EDGE_LOOP ( 'NONE', ( #10622, #19973, #25779, #5352 ) ) ;
#19693 = CARTESIAN_POINT ( 'NONE',  ( 18.55271417138208179, 18.55271417138200363, 12.99999999999999112 ) ) ;
#19694 = ADVANCED_FACE ( 'NONE', ( #24541 ), #10413, .T. ) ;
#19695 = CARTESIAN_POINT ( 'NONE',  ( 3.999999999999996003, -26.98750000000000426, 6.690598923241487306 ) ) ;
#19697 = ORIENTED_EDGE ( 'NONE', *, *, #1907, .T. ) ;
#19696 = CARTESIAN_POINT ( 'NONE',  ( 1.071796769724492338, 29.40759618943233278, 12.99999999999999467 ) ) ;
#19698 = CARTESIAN_POINT ( 'NONE',  ( -1.878215178124995832, 27.65312499938548640, 5.746835883940462963 ) ) ;
#19700 = CARTESIAN_POINT ( 'NONE',  ( -3.401318489841309578, -30.91344420362545264, -6.500000000000000000 ) ) ;
#19699 = AXIS2_PLACEMENT_3D ( 'NONE', #2786, #5149, #16794 ) ;
#19701 = VERTEX_POINT ( 'NONE', #14618 ) ;
#19702 = CARTESIAN_POINT ( 'NONE',  ( 0.000000000000000000, 0.000000000000000000, 1.000000000000000000 ) ) ;
#19703 = VERTEX_POINT ( 'NONE', #12785 ) ;
#19704 = ORIENTED_EDGE ( 'NONE', *, *, #5627, .F. ) ;
#19705 = CARTESIAN_POINT ( 'NONE',  ( 1.878215178124998275, 25.51562499938548711, 12.25316411605952283 ) ) ;
#19706 = AXIS2_PLACEMENT_3D ( 'NONE', #24989, #10859, #24742 ) ;
#19707 = EDGE_CURVE ( 'NONE', #24890, #1173, #18796, .T. ) ;
#19708 = CARTESIAN_POINT ( 'NONE',  ( 1.878215178125004048, -5.746835883940462963, 3.365624999385481875 ) ) ;
#19709 = EDGE_CURVE ( 'NONE', #17641, #345, #4555, .T. ) ;
#19710 = CARTESIAN_POINT ( 'NONE',  ( 27.49048467073848911, -14.54246377227368647, -6.500000000000000000 ) ) ;
#19711 =( LENGTH_UNIT ( ) NAMED_UNIT ( * ) SI_UNIT ( .MILLI., .METRE. ) );
#19712 = EDGE_CURVE ( 'NONE', #7736, #2329, #21453, .T. ) ;
#19713 = CARTESIAN_POINT ( 'NONE',  ( -30.45149776762720961, 6.317933499823766397, -2.750000000000000000 ) ) ;
#19714 = ADVANCED_FACE ( 'NONE', ( #20072 ), #17737, .T. ) ;
#19715 = CARTESIAN_POINT ( 'NONE',  ( 3.469446951953614189E-15, 30.00000000000000355, 8.999999999999992895 ) ) ;
#19716 = AXIS2_PLACEMENT_3D ( 'NONE', #5358, #21187, #1703 ) ;
#19717 = CARTESIAN_POINT ( 'NONE',  ( -29.62293631110035363, 7.734255490827311341, 1.000000000000000000 ) ) ;
#19718 =( BOUNDED_CURVE ( )  B_SPLINE_CURVE ( 2, ( #21928, #4008, #11974, #24135, #13573, #6097, #14080, #4129, #20084, #21539, #12108, #14733, #12492, #16445, #2815, #10654, #6743, #6485, #22185, #14591, #18530, #617, #10778, #20737, #24523, #12243, #4271, #18648, #2427, #12766, #8317, #18389, #10389, #8700, #12637, #14351, #20212, #20335, #14471, #2312, #731, #16305, #347, #16686, #10267, #6605, #24657, #22710, #4791, #22575, #18771, #18261, #862, #8842, #8583, #24273, #6360, #16829, #22313, #4391, #12371, #6220, #487, #16563, #8458, #24410, #14212, #22436, #4514, #2565, #20468, #10533, #20608, #4655, #2695, #19412, #1505, #9476, #23211, #11168, #23096, #13412, #17342, #15122, #11049, #25046, #15246, #5295, #19029, #3199, #19285, #23335, #15363, #3327, #1384, #22957, #9226, #24793, #2954, #13274, #19151, #1242, #10918, #7135, #3083, #12885, #17215, #4907, #7268, #21247, #16951, #1112, #6875, #14858, #5180, #9087, #18912, #11306, #22833, #25185, #9359 ),
 .UNSPECIFIED., .F., .F. ) 
 B_SPLINE_CURVE_WITH_KNOTS ( ( 3, 2, 2, 2, 2, 2, 2, 2, 2, 2, 2, 2, 2, 2, 2, 2, 2, 2, 2, 2, 2, 2, 2, 2, 2, 2, 2, 2, 2, 2, 2, 2, 2, 2, 2, 2, 2, 2, 2, 2, 2, 2, 2, 2, 2, 2, 2, 2, 2, 2, 2, 2, 2, 2, 2, 2, 2, 2, 2, 2, 3 ),
 ( 0.000000000000000000, 0.01666666666666666644, 0.03333333333333333287, 0.05000000000000000278, 0.06666666666666666574, 0.08333333333333332871, 0.1000000000000000056, 0.1166666666666666685, 0.1333333333333333315, 0.1499999999999999944, 0.1666666666666666574, 0.1833333333333333204, 0.2000000000000000111, 0.2166666666666666741, 0.2333333333333333370, 0.2500000000000000000, 0.2666666666666666630, 0.2833333333333333259, 0.2999999999999999889, 0.3166666666666666519, 0.3333333333333333148, 0.3499999999999999778, 0.3666666666666666408, 0.3833333333333333592, 0.4000000000000000222, 0.4166666666666666852, 0.4333333333333333481, 0.4500000000000000111, 0.4666666666666666741, 0.4833333333333333370, 0.5000000000000000000, 0.5166666666666667185, 0.5333333333333333259, 0.5500000000000000444, 0.5666666666666666519, 0.5833333333333333703, 0.5999999999999999778, 0.6166666666666666963, 0.6333333333333333037, 0.6500000000000000222, 0.6666666666666666297, 0.6833333333333333481, 0.6999999999999999556, 0.7166666666666666741, 0.7333333333333332815, 0.7500000000000000000, 0.7666666666666667185, 0.7833333333333333259, 0.8000000000000000444, 0.8166666666666666519, 0.8333333333333333703, 0.8499999999999999778, 0.8666666666666666963, 0.8833333333333333037, 0.9000000000000000222, 0.9166666666666666297, 0.9333333333333333481, 0.9499999999999999556, 0.9666666666666666741, 0.9833333333333332815, 1.000000000000000000 ),
 .UNSPECIFIED. ) 
 CURVE ( )  GEOMETRIC_REPRESENTATION_ITEM ( )  RATIONAL_B_SPLINE_CURVE ( ( 1.000000000000000000, 0.8660254037844387076, 1.000000000000000000, 0.8660254037844387076, 1.000000000000000000, 0.8660254037844387076, 1.000000000000000000, 0.8660254037844387076, 1.000000000000000000, 0.8660254037844387076, 1.000000000000000000, 0.8660254037844387076, 1.000000000000000000, 0.8660254037844387076, 1.000000000000000000, 0.8660254037844387076, 1.000000000000000000, 0.8660254037844387076, 1.000000000000000000, 0.8660254037844387076, 1.000000000000000000, 0.8660254037844387076, 1.000000000000000000, 0.8660254037844387076, 1.000000000000000000, 0.8660254037844387076, 1.000000000000000000, 0.8660254037844387076, 1.000000000000000000, 0.8660254037844387076, 1.000000000000000000, 0.8660254037844387076, 1.000000000000000000, 0.8660254037844387076, 1.000000000000000000, 0.8660254037844387076, 1.000000000000000000, 0.8660254037844387076, 1.000000000000000000, 0.8660254037844387076, 1.000000000000000000, 0.8660254037844387076, 1.000000000000000000, 0.8660254037844387076, 1.000000000000000000, 0.8660254037844387076, 1.000000000000000000, 0.8660254037844387076, 1.000000000000000000, 0.8660254037844387076, 1.000000000000000000, 0.8660254037844387076, 1.000000000000000000, 0.8660254037844387076, 1.000000000000000000, 0.8660254037844387076, 1.000000000000000000, 0.8660254037844387076, 1.000000000000000000, 0.8660254037844387076, 1.000000000000000000, 0.8660254037844387076, 1.000000000000000000, 0.8660254037844387076, 1.000000000000000000, 0.8660254037844387076, 1.000000000000000000, 0.8660254037844387076, 1.000000000000000000, 0.8660254037844387076, 1.000000000000000000, 0.8660254037844387076, 1.000000000000000000, 0.8660254037844387076, 1.000000000000000000, 0.8660254037844387076, 1.000000000000000000, 0.8660254037844387076, 1.000000000000000000, 0.8660254037844387076, 1.000000000000000000, 0.8660254037844387076, 1.000000000000000000, 0.8660254037844387076, 1.000000000000000000, 0.8660254037844387076, 1.000000000000000000, 0.8660254037844387076, 1.000000000000000000, 0.8660254037844387076, 1.000000000000000000, 0.8660254037844387076, 1.000000000000000000, 0.8660254037844387076, 1.000000000000000000, 0.8660254037844387076, 1.000000000000000000, 0.8660254037844387076, 1.000000000000000000, 0.8660254037844387076, 1.000000000000000000, 0.8660254037844387076, 1.000000000000000000, 0.8660254037844387076, 1.000000000000000000, 0.8660254037844387076, 1.000000000000000000, 0.8660254037844387076, 1.000000000000000000, 0.8660254037844387076, 1.000000000000000000, 0.8660254037844387076, 1.000000000000000000, 0.8660254037844387076, 1.000000000000000000, 0.8660254037844387076, 1.000000000000000000, 0.8660254037844387076, 1.000000000000000000, 0.8660254037844387076, 1.000000000000000000 ) ) 
 REPRESENTATION_ITEM ( '' )  );
#19719 = CARTESIAN_POINT ( 'NONE',  ( -3.999999999999997335, 27.00624999877096855, 11.30940107675849404 ) ) ;
#19720 = DIRECTION ( 'NONE',  ( 0.000000000000000000, -0.000000000000000000, 1.000000000000000000 ) ) ;
#19721 = CARTESIAN_POINT ( 'NONE',  ( 19.42333939484895211, 16.59491227010269299, 5.535898384862238508 ) ) ;
#19722 = ORIENTED_EDGE ( 'NONE', *, *, #14474, .F. ) ;
#19723 = CARTESIAN_POINT ( 'NONE',  ( 28.14012133169324414, 13.24173596767369254, 1.000000000000000000 ) ) ;
#19724 = CARTESIAN_POINT ( 'NONE',  ( -30.63887302793240508, 5.335677986745116286, -2.750000000000000000 ) ) ;
#19725 = AXIS2_PLACEMENT_3D ( 'NONE', #9895, #25727, #12117 ) ;
#19726 = CARTESIAN_POINT ( 'NONE',  ( -3.756430356249995661, 27.24062499938548498, 6.831223922626973533 ) ) ;
#19727 = AXIS2_PLACEMENT_3D ( 'NONE', #19487, #5752, #1582 ) ;
#19728 = CARTESIAN_POINT ( 'NONE',  ( 3.469446951953614189E-15, 40.00000000000000000, 8.999999999999992895 ) ) ;
#19729 = CARTESIAN_POINT ( 'NONE',  ( -3.999999999999996447, 26.16250000000000497, 11.30940107675849404 ) ) ;
#19730 = PLANE ( 'NONE',  #2639 ) ;
#19731 = EDGE_LOOP ( 'NONE', ( #8761, #1871, #23404, #18322 ) ) ;
#19732 = CARTESIAN_POINT ( 'NONE',  ( 0.000000000000000000, 29.64062499938549422, 13.33755215474602984 ) ) ;
#19733 = DIRECTION ( 'NONE',  ( 0.000000000000000000, 0.000000000000000000, -1.000000000000000000 ) ) ;
#19735 = ORIENTED_EDGE ( 'NONE', *, *, #23772, .T. ) ;
#19734 = PLANE ( 'NONE',  #17104 ) ;
#19736 = ORIENTED_EDGE ( 'NONE', *, *, #3624, .F. ) ;
#19737 = EDGE_LOOP ( 'NONE', ( #9568, #24171 ) ) ;
#19738 = VERTEX_POINT ( 'NONE', #18138 ) ;
#19739 = EDGE_LOOP ( 'NONE', ( #17307, #6420, #9475, #15467 ) ) ;
#19740 = CYLINDRICAL_SURFACE ( 'NONE', #23927, 4.000000000000000000 ) ;
#19741 = FACE_OUTER_BOUND ( 'NONE', #13858, .T. ) ;
#19742 = CIRCLE ( 'NONE', #9315, 0.4999999999999999445 ) ;
#19743 =( NAMED_UNIT ( * ) SI_UNIT ( $, .STERADIAN. ) SOLID_ANGLE_UNIT ( ) );
#19744 = CARTESIAN_POINT ( 'NONE',  ( -3.756430356249996105, 27.12812499938548783, 6.831223922626973533 ) ) ;
#19745 = VECTOR ( 'NONE', #24067, 1000.000000000000000 ) ;
#19746 = CARTESIAN_POINT ( 'NONE',  ( -3.756430356249997882, -11.16877607737301226, 3.103124999385483029 ) ) ;
#19747 = CARTESIAN_POINT ( 'NONE',  ( 2.000000000000000888, -12.46410161513774817, 4.368749998770966592 ) ) ;
#19748 = DIRECTION ( 'NONE',  ( 0.000000000000000000, 0.000000000000000000, 1.000000000000000000 ) ) ;
#19749 = EDGE_CURVE ( 'NONE', #24155, #25772, #2174, .T. ) ;
#19750 = CARTESIAN_POINT ( 'NONE',  ( -1.878215178124995832, 28.10312499938548569, 5.746835883940462963 ) ) ;
#19751 = EDGE_CURVE ( 'NONE', #16500, #1701, #25036, .T. ) ;
#19752 = DIRECTION ( 'NONE',  ( 0.000000000000000000, 0.000000000000000000, 1.000000000000000000 ) ) ;
#19753 = FACE_OUTER_BOUND ( 'NONE', #1896, .T. ) ;
#19754 = CARTESIAN_POINT ( 'NONE',  ( 2.000000000000003997, -5.535898384862238508, 1.875000000000001776 ) ) ;
#19755 = DIRECTION ( 'NONE',  ( 1.000000000000000000, 0.000000000000000000, 0.000000000000000000 ) ) ;
#19756 = FACE_OUTER_BOUND ( 'NONE', #20540, .T. ) ;
#19757 = CARTESIAN_POINT ( 'NONE',  ( 20.43330379829292198, 15.12090904237410527, 8.999999999999992895 ) ) ;
#19758 = CARTESIAN_POINT ( 'NONE',  ( -2.000000000000003997, -27.71874999877097068, 5.535898384862238508 ) ) ;
#19759 = ADVANCED_FACE ( 'NONE', ( #19690, #212, #23492 ), #21789, .T. ) ;
#19760 = CARTESIAN_POINT ( 'NONE',  ( 3.756430356250004099, 27.09062499938548285, 6.831223922626973533 ) ) ;
#19761 = CARTESIAN_POINT ( 'NONE',  ( 3.918623196469464443, 34.50000000000000000, 4.456389954662532737 ) ) ;
#19762 = COLOUR_RGB ( '',0.8941176470588234615, 0.8941176470588234615, 0.8941176470588234615 ) ;
#19763 = DIRECTION ( 'NONE',  ( -0.000000000000000000, 1.000000000000000000, -0.000000000000000000 ) ) ;
#19764 = ORIENTED_EDGE ( 'NONE', *, *, #15482, .F. ) ;
#19765 = CYLINDRICAL_SURFACE ( 'NONE', #6235, 5.500000000000000000 ) ;
#19766 = VERTEX_POINT ( 'NONE', #17862 ) ;
#19767 =( BOUNDED_CURVE ( )  B_SPLINE_CURVE ( 2, ( #1152, #25342, #25606, #15409, #3124, #1545, #21166, #7422, #23382 ),
 .UNSPECIFIED., .F., .F. ) 
 B_SPLINE_CURVE_WITH_KNOTS ( ( 3, 2, 2, 2, 3 ),
 ( 0.3750000000000000000, 0.3833333333333333592, 0.4000000000000000222, 0.4166666666666666852, 0.4250000000000000444 ),
 .UNSPECIFIED. ) 
 CURVE ( )  GEOMETRIC_REPRESENTATION_ITEM ( )  RATIONAL_B_SPLINE_CURVE ( ( 0.9330127018922194093, 0.9330127018922194093, 1.000000000000000000, 0.8660254037844387076, 1.000000000000000000, 0.8660254037844387076, 1.000000000000000000, 0.9330127018922191873, 0.9330127018922194093 ) ) 
 REPRESENTATION_ITEM ( '' )  );
#19768 = ORIENTED_EDGE ( 'NONE', *, *, #9599, .F. ) ;
#19769 = DIRECTION ( 'NONE',  ( 0.000000000000000000, 0.000000000000000000, 1.000000000000000000 ) ) ;
#19770 = EDGE_LOOP ( 'NONE', ( #16854, #2458, #17964, #11796 ) ) ;
#19771 = CARTESIAN_POINT ( 'NONE',  ( -1.878215178125000939, -28.77812499938548640, 12.25316411605952283 ) ) ;
#19772 = VERTEX_POINT ( 'NONE', #25833 ) ;
#19773 = FACE_OUTER_BOUND ( 'NONE', #13091, .T. ) ;
#19774 =( BOUNDED_CURVE ( )  B_SPLINE_CURVE ( 2, ( #15180, #1438, #6928, #18835, #23148, #5228, #4966, #13207, #13331 ),
 .UNSPECIFIED., .F., .F. ) 
 B_SPLINE_CURVE_WITH_KNOTS ( ( 3, 2, 2, 2, 3 ),
 ( 0.7750000000000000222, 0.7833333333333333259, 0.8000000000000000444, 0.8166666666666666519, 0.8249999999999999556 ),
 .UNSPECIFIED. ) 
 CURVE ( )  GEOMETRIC_REPRESENTATION_ITEM ( )  RATIONAL_B_SPLINE_CURVE ( ( 0.9330127018922194093, 0.9330127018922194093, 1.000000000000000000, 0.8660254037844387076, 1.000000000000000000, 0.8660254037844387076, 1.000000000000000000, 0.9330127018922198534, 0.9330127018922194093 ) ) 
 REPRESENTATION_ITEM ( '' )  );
#19775 = VERTEX_POINT ( 'NONE', #21525 ) ;
#19776 = CARTESIAN_POINT ( 'NONE',  ( 4.000000000000001776, 26.31250000000000000, 11.30940107675849760 ) ) ;
#19777 = CARTESIAN_POINT ( 'NONE',  ( 1.859271017917182139E-15, 29.38750000000000639, 12.99999999999999289 ) ) ;
#19778 = DIRECTION ( 'NONE',  ( 0.1253332335643120576, 0.9921147013144768767, 0.000000000000000000 ) ) ;
#19779 = CARTESIAN_POINT ( 'NONE',  ( 1.071796769724495446, 25.99240381056766935, 4.999999999999992895 ) ) ;
#19780 = CARTESIAN_POINT ( 'NONE',  ( 17.61346044605677008, 22.92585520197544469, 11.16877607737301226 ) ) ;
#19781 = CARTESIAN_POINT ( 'NONE',  ( 0.000000000000000000, 0.000000000000000000, 1.000000000000000000 ) ) ;
#19782 = ADVANCED_FACE ( 'NONE', ( #3871 ), #1790, .T. ) ;
#19783 = CARTESIAN_POINT ( 'NONE',  ( 3.959305671612554781E-15, 31.50000000000000000, 12.99999999999999289 ) ) ;
#19784 = CARTESIAN_POINT ( 'NONE',  ( 2.000000000000003997, 29.12500000000000000, 5.535898384862238508 ) ) ;
#19785 = CARTESIAN_POINT ( 'NONE',  ( 0.000000000000000000, 0.000000000000000000, 1.000000000000000000 ) ) ;
#19786 = CYLINDRICAL_SURFACE ( 'NONE', #15424, 0.5000000000000004441 ) ;
#19787 = VERTEX_POINT ( 'NONE', #15905 ) ;
#19788 = VERTEX_POINT ( 'NONE', #15769 ) ;
#19789 = CARTESIAN_POINT ( 'NONE',  ( 1.878215178125001605, 26.07812499938549067, 12.25316411605952283 ) ) ;
#19790 = EDGE_CURVE ( 'NONE', #4065, #24402, #9758, .T. ) ;
#19791 = ORIENTED_EDGE ( 'NONE', *, *, #4612, .F. ) ;
#19792 = CARTESIAN_POINT ( 'NONE',  ( -1.999999999999998224, 26.14374999877096784, 12.46410161513774639 ) ) ;
#19793 = CARTESIAN_POINT ( 'NONE',  ( -3.756430356249995661, 26.79062499938548925, 6.831223922626973533 ) ) ;
#19794 = CARTESIAN_POINT ( 'NONE',  ( 18.68225429291731743, 24.86329371854767700, -6.500000000000000000 ) ) ;
#19795 = EDGE_LOOP ( 'NONE', ( #1383, #17696 ) ) ;
#19796 = VERTEX_POINT ( 'NONE', #5823 ) ;
#19797 = CARTESIAN_POINT ( 'NONE',  ( -1.071796769724488785, 26.16115380933863577, 12.99999999999999289 ) ) ;
#19798 = VERTEX_POINT ( 'NONE', #13945 ) ;
#19799 = CARTESIAN_POINT ( 'NONE',  ( 0.4972522109372495280, 38.55547752541761497, 14.92368914124902801 ) ) ;
#19800 = LINE ( 'NONE', #7897, #18453 ) ;
#19801 = CARTESIAN_POINT ( 'NONE',  ( -3.756430356249994773, 27.16562499938548214, 8.999999999999992895 ) ) ;
#19802 = CARTESIAN_POINT ( 'NONE',  ( -29.41953157733101065, -10.08469938919468945, -6.500000000000000000 ) ) ;
#19803 = CARTESIAN_POINT ( 'NONE',  ( 4.000000000000001776, 25.90000000000000568, 8.999999999999992895 ) ) ;
#19804 = CARTESIAN_POINT ( 'NONE',  ( -1.878215178124998497, 26.34062499938548285, 12.25316411605951927 ) ) ;
#19805 =( NAMED_UNIT ( * ) PLANE_ANGLE_UNIT ( ) SI_UNIT ( $, .RADIAN. ) );
#19806 = CARTESIAN_POINT ( 'NONE',  ( -1.999999999999998224, 27.55000000000000071, 12.46410161513774639 ) ) ;
#19807 = EDGE_CURVE ( 'NONE', #19911, #5263, #6257, .T. ) ;
#19808 = CYLINDRICAL_SURFACE ( 'NONE', #16243, 0.5000000000000002220 ) ;
#19809 = CARTESIAN_POINT ( 'NONE',  ( 15.93641908099185933, 21.59327333048416975, 6.690598923241487306 ) ) ;
#19810 = CARTESIAN_POINT ( 'NONE',  ( 20.48178985837210320, 20.48178985837202859, 4.662447845253954171 ) ) ;
#19811 = CARTESIAN_POINT ( 'NONE',  ( -3.063240906311874401, -29.84319947910909931, 11.57226653943513028 ) ) ;
#19812 = CARTESIAN_POINT ( 'NONE',  ( 3.469446951953614189E-15, 40.00000000000000000, 8.999999999999992895 ) ) ;
#19813 = CARTESIAN_POINT ( 'NONE',  ( -4.648177544792955347E-16, 27.08124999877097139, 12.99999999999999289 ) ) ;
#19814 = DIRECTION ( 'NONE',  ( -0.000000000000000000, -0.000000000000000000, -1.000000000000000000 ) ) ;
#19815 = DIRECTION ( 'NONE',  ( 0.000000000000000000, 0.000000000000000000, -1.000000000000000000 ) ) ;
#19816 = ORIENTED_EDGE ( 'NONE', *, *, #1933, .T. ) ;
#19817 = CARTESIAN_POINT ( 'NONE',  ( 4.000000000000003553, 28.09374999877097068, 8.999999999999992895 ) ) ;
#19818 = CARTESIAN_POINT ( 'NONE',  ( 3.999999999999997335, -26.61250000000000071, 11.30940107675849404 ) ) ;
#19820 = VERTEX_POINT ( 'NONE', #721 ) ;
#19819 = CARTESIAN_POINT ( 'NONE',  ( 3.756430356250004099, 25.29062499938548925, 6.831223922626973533 ) ) ;
#19821 = CARTESIAN_POINT ( 'NONE',  ( 3.756430356250003655, 27.50312499938548427, 8.999999999999992895 ) ) ;
#19822 = CARTESIAN_POINT ( 'NONE',  ( 3.999999999999996447, -29.66874999877096997, 8.999999999999992895 ) ) ;
#19823 = EDGE_LOOP ( 'NONE', ( #13528, #24643, #16899, #24425 ) ) ;
#19824 = CARTESIAN_POINT ( 'NONE',  ( 30.91344420362545975, -3.401318489841208326, -2.750000000000000000 ) ) ;
#19825 = ORIENTED_EDGE ( 'NONE', *, *, #21823, .F. ) ;
#19826 = VERTEX_POINT ( 'NONE', #12357 ) ;
#19827 = CARTESIAN_POINT ( 'NONE',  ( -1.878215178124994722, 25.29062499938548925, 5.746835883940462963 ) ) ;
#19828 = CARTESIAN_POINT ( 'NONE',  ( 1.878215178125004048, -5.746835883940462963, 4.265624999385483562 ) ) ;
#19829 = SHAPE_REPRESENTATION ( 'stem', ( #21036 ), #5183 ) ;
#19830 = CARTESIAN_POINT ( 'NONE',  ( -1.999999999999998224, 27.49374999877096926, 12.46410161513774639 ) ) ;
#19831 = EDGE_CURVE ( 'NONE', #9030, #6676, #5252, .T. ) ;
#19832 = CARTESIAN_POINT ( 'NONE',  ( 2.000000000000000888, -12.46410161513774817, 3.974999999999999201 ) ) ;
#19833 = LINE ( 'NONE', #25728, #9636 ) ;
#19834 = CARTESIAN_POINT ( 'NONE',  ( 18.28012134629595309, 25.16042852506084770, -6.500000000000000000 ) ) ;
#19835 = DIRECTION ( 'NONE',  ( 0.000000000000000000, 0.000000000000000000, 1.000000000000000000 ) ) ;
#19836 = CARTESIAN_POINT ( 'NONE',  ( 19.33937046545212013, 22.16779759019823359, 12.46410161513774639 ) ) ;
#19837 = CARTESIAN_POINT ( 'NONE',  ( 15.59820611967510295, 20.91060087559377934, 8.999999999999992895 ) ) ;
#19838 = CARTESIAN_POINT ( 'NONE',  ( 15.28676472490765548, 20.94361897439997122, 8.999999999999992895 ) ) ;
#19839 = ORIENTED_EDGE ( 'NONE', *, *, #8937, .T. ) ;
#19840 = FACE_OUTER_BOUND ( 'NONE', #4224, .T. ) ;
#19841 = CARTESIAN_POINT ( 'NONE',  ( 5.242549070241824261, 39.00275152493676245, 7.344768029949470645 ) ) ;
#19842 = CARTESIAN_POINT ( 'NONE',  ( 3.756430356250003655, 27.95312499938548711, 8.999999999999992895 ) ) ;
#19844 = EDGE_CURVE ( 'NONE', #11111, #10619, #10375, .T. ) ;
#19843 = DIRECTION ( 'NONE',  ( -0.000000000000000000, -1.000000000000000000, -0.000000000000000000 ) ) ;
#19845 = CARTESIAN_POINT ( 'NONE',  ( -3.469446951953614189E-15, -30.00000000000000355, 8.999999999999992895 ) ) ;
#19846 = CARTESIAN_POINT ( 'NONE',  ( 3.017230054654504556, 38.72260848564139479, 13.92749297489922355 ) ) ;
#19847 = ORIENTED_EDGE ( 'NONE', *, *, #12060, .T. ) ;
#19848 = LINE ( 'NONE', #887, #5083 ) ;
#19849 = CARTESIAN_POINT ( 'NONE',  ( 3.469446951953614189E-15, 40.00000000000000000, 8.999999999999992895 ) ) ;
#19851 = ORIENTED_EDGE ( 'NONE', *, *, #25005, .F. ) ;
#19850 = CARTESIAN_POINT ( 'NONE',  ( -4.000000000000001776, -26.31250000000000000, 11.30940107675849760 ) ) ;
#19852 = EDGE_CURVE ( 'NONE', #18040, #17840, #13359, .T. ) ;
#19853 = ORIENTED_EDGE ( 'NONE', *, *, #13998, .F. ) ;
#19854 = ORIENTED_EDGE ( 'NONE', *, *, #1541, .F. ) ;
#19855 = ADVANCED_FACE ( 'NONE', ( #20198 ), #6473, .T. ) ;
#19856 = ORIENTED_EDGE ( 'NONE', *, *, #8461, .F. ) ;
#19857 = CARTESIAN_POINT ( 'NONE',  ( -24.66042852506104310, -18.28012134629567598, 1.000000000000000000 ) ) ;
#19858 = CARTESIAN_POINT ( 'NONE',  ( 18.87091222291601866, 18.87091222291595827, 12.99999999999999289 ) ) ;
#19859 = DIRECTION ( 'NONE',  ( 0.000000000000000000, 0.000000000000000000, 1.000000000000000000 ) ) ;
#19860 = CARTESIAN_POINT ( 'NONE',  ( -3.756430356250000546, 26.30312499938548854, 11.16877607737301226 ) ) ;
#19861 = CIRCLE ( 'NONE', #12349, 31.10000000000000142 ) ;
#19862 = CARTESIAN_POINT ( 'NONE',  ( 1.878215178125004048, -5.746835883940462963, 2.915624999385482585 ) ) ;
#19863 = CARTESIAN_POINT ( 'NONE',  ( -1.999999999999995781, -5.535898384862237620, 4.143749998770966947 ) ) ;
#19864 = CARTESIAN_POINT ( 'NONE',  ( 1.878215178125004048, 27.12812499938548783, 5.746835883940462963 ) ) ;
#19865 = FACE_OUTER_BOUND ( 'NONE', #22770, .T. ) ;
#19866 = CARTESIAN_POINT ( 'NONE',  ( -1.999999999999998224, -12.46410161513774639, 0.7500000000000006661 ) ) ;
#19867 = CARTESIAN_POINT ( 'NONE',  ( -1.999999999999998224, -12.46410161513774639, 2.999999999999999112 ) ) ;
#19868 = FACE_OUTER_BOUND ( 'NONE', #12334, .T. ) ;
#19869 = CARTESIAN_POINT ( 'NONE',  ( 1.071796769724490783, 26.20134618820330630, 12.99999999999999467 ) ) ;
#19870 = FACE_OUTER_BOUND ( 'NONE', #25240, .T. ) ;
#19871 = CARTESIAN_POINT ( 'NONE',  ( -2.620986760973688460E-15, -29.78124999877096712, 13.61880215351699874 ) ) ;
#19872 = CARTESIAN_POINT ( 'NONE',  ( -3.756430356249996994, 28.17812499938548498, 8.999999999999992895 ) ) ;
#19873 = DIRECTION ( 'NONE',  ( 0.000000000000000000, 0.000000000000000000, 1.000000000000000000 ) ) ;
#19874 = CARTESIAN_POINT ( 'NONE',  ( -1.071796769724488563, 29.76115380933863364, 12.99999999999999289 ) ) ;
#19875 = DIRECTION ( 'NONE',  ( -0.000000000000000000, -0.000000000000000000, 1.000000000000000000 ) ) ;
#19876 = VERTEX_POINT ( 'NONE', #24259 ) ;
#19877 = DIRECTION ( 'NONE',  ( 0.000000000000000000, 0.000000000000000000, 1.000000000000000000 ) ) ;
#19879 = ORIENTED_EDGE ( 'NONE', *, *, #5087, .F. ) ;
#19878 = CARTESIAN_POINT ( 'NONE',  ( -1.878215178125000939, -29.11562499938548498, 12.25316411605952283 ) ) ;
#19880 = EDGE_LOOP ( 'NONE', ( #1478, #15917, #12273, #9416, #3968, #1702, #22854, #15595 ) ) ;
#19881 = CARTESIAN_POINT ( 'NONE',  ( 0.000000000000000000, 0.000000000000000000, -6.500000000000000000 ) ) ;
#19882 = VERTEX_POINT ( 'NONE', #24512 ) ;
#19883 = CARTESIAN_POINT ( 'NONE',  ( -3.756430356250002323, -29.26562499938548356, 11.16877607737301226 ) ) ;
#19884 = EDGE_CURVE ( 'NONE', #3918, #25139, #13417, .T. ) ;
#19885 = ORIENTED_EDGE ( 'NONE', *, *, #18494, .F. ) ;
#19886 = CARTESIAN_POINT ( 'NONE',  ( 2.000000000000003997, 25.46874999877096712, 5.535898384862238508 ) ) ;
#19887 = EDGE_CURVE ( 'NONE', #4092, #23536, #6594, .T. ) ;
#19888 = ORIENTED_EDGE ( 'NONE', *, *, #1809, .T. ) ;
#19889 = CARTESIAN_POINT ( 'NONE',  ( 2.000000000000000888, 28.97500000000000142, 12.46410161513774817 ) ) ;
#19890 = CARTESIAN_POINT ( 'NONE',  ( 3.756430356250003655, 27.05312499938548498, 8.999999999999992895 ) ) ;
#19891 = CARTESIAN_POINT ( 'NONE',  ( 2.672651547586948120E-15, -13.33755215474602984, 1.040624999385485472 ) ) ;
#19892 = CARTESIAN_POINT ( 'NONE',  ( 4.000000000000003553, -8.999999999999992895, 1.293749998770969079 ) ) ;
#19893 = CARTESIAN_POINT ( 'NONE',  ( 20.79998790990604718, 20.79998790990596902, 4.662447845253954171 ) ) ;
#19894 = CARTESIAN_POINT ( 'NONE',  ( -1.394453263437886604E-15, 27.30624999877096926, 4.999999999999991118 ) ) ;
#19895 = SURFACE_STYLE_FILL_AREA ( #2383 ) ;
#19896 = ITEM_DEFINED_TRANSFORMATION ( 'NONE', 'NONE', #11867,  #21036 ) ;
#19897 = CARTESIAN_POINT ( 'NONE',  ( -1.999999999999998224, 29.35000000000000142, 12.46410161513774639 ) ) ;
#19898 = CARTESIAN_POINT ( 'NONE',  ( 1.878215178125004048, -5.746835883940462963, 0.7781249993854856273 ) ) ;
#19899 = CARTESIAN_POINT ( 'NONE',  ( 19.60447174239884305, 22.26066912035814127, 12.25316411605951927 ) ) ;
#19900 = CARTESIAN_POINT ( 'NONE',  ( 27.09999999999999787, 0.6000000000000000888, 19.00000000000000000 ) ) ;
#19901 = ORIENTED_EDGE ( 'NONE', *, *, #14143, .T. ) ;
#19902 = VERTEX_POINT ( 'NONE', #14459 ) ;
#19903 = CARTESIAN_POINT ( 'NONE',  ( -1.878215178124998275, 26.30312499938548854, 5.746835883940462963 ) ) ;
#19904 =( BOUNDED_CURVE ( )  B_SPLINE_CURVE ( 2, ( #17808, #12167, #7735, #25773, #7854 ),
 .UNSPECIFIED., .F., .F. ) 
 B_SPLINE_CURVE_WITH_KNOTS ( ( 3, 2, 3 ),
 ( 0.000000000000000000, 0.01666666666666666644, 0.02500000000000000486 ),
 .UNSPECIFIED. ) 
 CURVE ( )  GEOMETRIC_REPRESENTATION_ITEM ( )  RATIONAL_B_SPLINE_CURVE ( ( 1.000000000000000000, 0.8660254037844387076, 1.000000000000000000, 0.9330127018922194093, 0.9330127018922194093 ) ) 
 REPRESENTATION_ITEM ( '' )  );
#19905 = ORIENTED_EDGE ( 'NONE', *, *, #16510, .F. ) ;
#19906 = CARTESIAN_POINT ( 'NONE',  ( -3.469446951953614189E-15, -30.00000000000000355, 8.999999999999992895 ) ) ;
#19907 = EDGE_CURVE ( 'NONE', #22503, #4122, #12478, .T. ) ;
#19908 = CARTESIAN_POINT ( 'NONE',  ( -3.999999999999996003, 29.63124999877096499, 6.690598923241487306 ) ) ;
#19909 = CARTESIAN_POINT ( 'NONE',  ( -3.756430356249996994, 29.07812499938548356, 8.999999999999992895 ) ) ;
#19910 = CARTESIAN_POINT ( 'NONE',  ( 17.75721904254721295, 17.75721904254714545, 4.999999999999992006 ) ) ;
#19911 = VERTEX_POINT ( 'NONE', #16433 ) ;
#19912 = EDGE_CURVE ( 'NONE', #16478, #2372, #16801, .T. ) ;
#19913 = CARTESIAN_POINT ( 'NONE',  ( 1.500000000000001776, -10.49999999999999289, 4.999999999999993783 ) ) ;
#19914 = ORIENTED_EDGE ( 'NONE', *, *, #20242, .F. ) ;
#19915 = CARTESIAN_POINT ( 'NONE',  ( 3.020711573345385315, 38.79236218548354032, 4.157123895590975060 ) ) ;
#19916 = CARTESIAN_POINT ( 'NONE',  ( -3.756430356249995661, 26.22812499938548214, 6.831223922626973533 ) ) ;
#19917 = FACE_OUTER_BOUND ( 'NONE', #6285, .T. ) ;
#19918 = DIRECTION ( 'NONE',  ( -0.7289686274214034478, 0.6845471059286972748, 0.000000000000000000 ) ) ;
#19919 = CARTESIAN_POINT ( 'NONE',  ( 1.071796769724487675, 29.53615380933863221, 4.999999999999988454 ) ) ;
#19920 = CARTESIAN_POINT ( 'NONE',  ( 6.009258394948636914E-15, 28.26250000000000639, 4.381197846482986158 ) ) ;
#19921 = EDGE_CURVE ( 'NONE', #11648, #7998, #5011, .T. ) ;
#19922 = CARTESIAN_POINT ( 'NONE',  ( -3.756430356249996994, 26.71562499938548285, 8.999999999999992895 ) ) ;
#19923 = FILL_AREA_STYLE ('',( #23995 ) ) ;
#19924 = DIRECTION ( 'NONE',  ( 0.000000000000000000, 1.000000000000000000, 0.000000000000000000 ) ) ;
#19925 = CARTESIAN_POINT ( 'NONE',  ( 0.000000000000000000, 0.000000000000000000, 1.000000000000000000 ) ) ;
#19926 = CARTESIAN_POINT ( 'NONE',  ( 17.20921128712764414, 22.86606553661995278, 6.690598923241487306 ) ) ;
#19927 = DIRECTION ( 'NONE',  ( 1.000000000000000000, 0.000000000000000000, 0.000000000000000000 ) ) ;
#19928 = CYLINDRICAL_SURFACE ( 'NONE', #13423, 4.000000000000000000 ) ;
#19929 = CARTESIAN_POINT ( 'NONE',  ( 3.999999999999997335, -27.90624999877097068, 11.30940107675849404 ) ) ;
#19930 = CARTESIAN_POINT ( 'NONE',  ( -3.735045420075836212E-15, -25.70312499938548001, 4.662447845253954171 ) ) ;
#19931 = AXIS2_PLACEMENT_3D ( 'NONE', #5339, #21675, #3760 ) ;
#19932 = B_SPLINE_CURVE_WITH_KNOTS ( 'NONE', 3,
 ( #19811, #17734, #19686, #7913, #21643, #6204, #10000, #9754 ),
 .UNSPECIFIED., .F., .F.,
 ( 4, 2, 2, 4 ),
 ( 0.01599790909976502723, 0.01669365098321972177, 0.01738939286667441630, 0.01878087663358380885 ),
 .UNSPECIFIED. ) ;
#19933 = DIRECTION ( 'NONE',  ( 0.000000000000000000, 0.000000000000000000, 1.000000000000000000 ) ) ;
#19934 = ORIENTED_EDGE ( 'NONE', *, *, #22393, .F. ) ;
#19935 = CARTESIAN_POINT ( 'NONE',  ( -3.999999999999996003, 27.83124999877096784, 6.690598923241487306 ) ) ;
#19936 = CARTESIAN_POINT ( 'NONE',  ( -4.000000000000003553, -27.70000000000000284, 8.999999999999992895 ) ) ;
#19938 = ORIENTED_EDGE ( 'NONE', *, *, #539, .T. ) ;
#19937 = CARTESIAN_POINT ( 'NONE',  ( -1.878215178124998275, 27.35312499938548925, 12.25316411605951927 ) ) ;
#19939 = EDGE_CURVE ( 'NONE', #18585, #10164, #24397, .T. ) ;
#19940 = CARTESIAN_POINT ( 'NONE',  ( -1.878215178124998497, 27.35312499938548569, 12.25316411605951927 ) ) ;
#19941 = DIRECTION ( 'NONE',  ( 0.000000000000000000, 0.000000000000000000, 1.000000000000000000 ) ) ;
#19942 = DIRECTION ( 'NONE',  ( 0.000000000000000000, 0.000000000000000000, 1.000000000000000000 ) ) ;
#19943 = DIRECTION ( 'NONE',  ( -1.000000000000000000, 0.000000000000000000, -0.000000000000000000 ) ) ;
#19944 = VERTEX_POINT ( 'NONE', #20727 ) ;
#19945 = ORIENTED_EDGE ( 'NONE', *, *, #20774, .T. ) ;
#19946 = CARTESIAN_POINT ( 'NONE',  ( 6.317933499823313426, 30.45149776762729843, 1.000000000000000000 ) ) ;
#19947 = CARTESIAN_POINT ( 'NONE',  ( -3.756430356249996549, 26.71562499938548996, 8.999999999999992895 ) ) ;
#19948 = EDGE_CURVE ( 'NONE', #10075, #15562, #18356, .T. ) ;
#19949 = CARTESIAN_POINT ( 'NONE',  ( 1.878215178125004048, -5.746835883940462963, 3.815624999385484273 ) ) ;
#19950 = EDGE_CURVE ( 'NONE', #7429, #24918, #7258, .T. ) ;
#19951 = AXIS2_PLACEMENT_3D ( 'NONE', #17924, #3666, #11644 ) ;
#19952 = DIRECTION ( 'NONE',  ( -0.000000000000000000, -0.000000000000000000, 1.000000000000000000 ) ) ;
#19953 = CARTESIAN_POINT ( 'NONE',  ( -13.69242354489114177, 27.92360179968391165, 1.000000000000000000 ) ) ;
#19954 = CARTESIAN_POINT ( 'NONE',  ( 3.469446951953614189E-15, 38.49999999999999289, 8.999999999999992895 ) ) ;
#19955 = CARTESIAN_POINT ( 'NONE',  ( 4.000000000000005329, 29.48124999877097707, 6.690598923241489970 ) ) ;
#19956 = AXIS2_PLACEMENT_3D ( 'NONE', #7081, #25513, #9433 ) ;
#19957 = CARTESIAN_POINT ( 'NONE',  ( -18.28012134629558716, 25.16042852506110705, -6.500000000000000000 ) ) ;
#19958 = FACE_OUTER_BOUND ( 'NONE', #6095, .T. ) ;
#19959 = CARTESIAN_POINT ( 'NONE',  ( 19.37037015225818948, 16.71417277429875625, 12.25316411605952283 ) ) ;
#19960 = CARTESIAN_POINT ( 'NONE',  ( 17.16943652981684210, 22.82629077930915074, 6.690598923241487306 ) ) ;
#19961 = ORIENTED_EDGE ( 'NONE', *, *, #19712, .T. ) ;
#19962 = CARTESIAN_POINT ( 'NONE',  ( -5.345872705005824344, 38.71721868403346178, 11.20510013807279037 ) ) ;
#19963 = CARTESIAN_POINT ( 'NONE',  ( -27.25313774936430633, -14.98253926456308172, -6.500000000000000000 ) ) ;
#19964 = CARTESIAN_POINT ( 'NONE',  ( 1.878215178125004048, 28.02812499938548640, 5.746835883940462963 ) ) ;
#19965 = CARTESIAN_POINT ( 'NONE',  ( -3.015186248472646824, 29.84868090056883716, 11.64163568064553544 ) ) ;
#19966 = CARTESIAN_POINT ( 'NONE',  ( -1.999999999999994893, 26.05000000000000426, 5.535898384862237620 ) ) ;
#19967 = FACE_OUTER_BOUND ( 'NONE', #12528, .T. ) ;
#19968 = VERTEX_POINT ( 'NONE', #25035 ) ;
#19969 = CARTESIAN_POINT ( 'NONE',  ( 2.000000000000003997, 27.26874999877097139, 5.535898384862238508 ) ) ;
#19970 = CARTESIAN_POINT ( 'NONE',  ( -1.999999999999995781, 25.54374999877096997, 5.535898384862237620 ) ) ;
#19971 = DIRECTION ( 'NONE',  ( 0.000000000000000000, 0.000000000000000000, 1.000000000000000000 ) ) ;
#19973 = ORIENTED_EDGE ( 'NONE', *, *, #10506, .F. ) ;
#19972 = DIRECTION ( 'NONE',  ( 0.000000000000000000, 0.000000000000000000, 1.000000000000000000 ) ) ;
#19974 = CIRCLE ( 'NONE', #9120, 0.5000000000000001110 ) ;
#19975 = ORIENTED_EDGE ( 'NONE', *, *, #23543, .F. ) ;
#19976 = ORIENTED_EDGE ( 'NONE', *, *, #17786, .F. ) ;
#19977 = CIRCLE ( 'NONE', #15815, 0.5000000000000001110 ) ;
#19978 = EDGE_LOOP ( 'NONE', ( #17779, #553, #163, #17327 ) ) ;
#19979 = DIRECTION ( 'NONE',  ( 0.000000000000000000, 0.000000000000000000, 1.000000000000000000 ) ) ;
#19980 = CIRCLE ( 'NONE', #3708, 0.5000000000000004441 ) ;
#19981 = EDGE_CURVE ( 'NONE', #19352, #19279, #13262, .T. ) ;
#19982 = AXIS2_PLACEMENT_3D ( 'NONE', #12750, #7470, #20721 ) ;
#19983 = DIRECTION ( 'NONE',  ( 0.000000000000000000, 0.000000000000000000, 1.000000000000000000 ) ) ;
#19984 = CARTESIAN_POINT ( 'NONE',  ( -3.756430356249994773, 27.16562499938548214, 8.999999999999992895 ) ) ;
#19985 = ADVANCED_FACE ( 'NONE', ( #9078 ), #9351, .T. ) ;
#19986 = DIRECTION ( 'NONE',  ( 0.9510565162951586382, 0.3090169943749320192, 0.000000000000000000 ) ) ;
#19987 = CARTESIAN_POINT ( 'NONE',  ( -3.999999999999997335, -11.30940107675849404, 4.256249998770964105 ) ) ;
#19988 = CARTESIAN_POINT ( 'NONE',  ( 1.878215178125000939, 25.96562499938548285, 12.25316411605952283 ) ) ;
#19989 = CARTESIAN_POINT ( 'NONE',  ( 27.00874656207304980, 15.41874213889405176, 1.000000000000000000 ) ) ;
#19990 = VECTOR ( 'NONE', #16752, 1000.000000000000000 ) ;
#19991 = CYLINDRICAL_SURFACE ( 'NONE', #15540, 4.000000000000000000 ) ;
#19992 = CARTESIAN_POINT ( 'NONE',  ( -3.756430356249997438, 26.75312499938548427, 11.16877607737301048 ) ) ;
#19993 = AXIS2_PLACEMENT_3D ( 'NONE', #16936, #11035, #9207 ) ;
#19994 = DIRECTION ( 'NONE',  ( -0.8443279255020205154, -0.5358267949789882190, 0.000000000000000000 ) ) ;
#19996 = EDGE_CURVE ( 'NONE', #22681, #1345, #8965, .T. ) ;
#19995 = FACE_OUTER_BOUND ( 'NONE', #4304, .T. ) ;
#19997 = CARTESIAN_POINT ( 'NONE',  ( 2.000000000000000000, 27.62500000000000355, 12.46410161513774817 ) ) ;
#19998 = CARTESIAN_POINT ( 'NONE',  ( 3.999999999999997335, -28.80624999877096926, 11.30940107675849404 ) ) ;
#19999 = CARTESIAN_POINT ( 'NONE',  ( -3.756430356249996994, 27.72812499938548569, 8.999999999999992895 ) ) ;
#20000 = AXIS2_PLACEMENT_3D ( 'NONE', #24519, #10262, #14588 ) ;
#20001 = CARTESIAN_POINT ( 'NONE',  ( 0.5000000000000001110, 6.123233995736767268E-17, 20.00000000000000000 ) ) ;
#20003 = CARTESIAN_POINT ( 'NONE',  ( 4.000000000000003553, -8.999999999999992895, 1.743749998770967924 ) ) ;
#20002 = CIRCLE ( 'NONE', #2465, 31.10000000000000142 ) ;
#20004 = CARTESIAN_POINT ( 'NONE',  ( 1.071796769724487230, -25.97634618820330132, 4.999999999999992006 ) ) ;
#20005 = ORIENTED_EDGE ( 'NONE', *, *, #2230, .T. ) ;
#20006 = CARTESIAN_POINT ( 'NONE',  ( -3.999999999999996447, -8.999999999999992895, 1.574999999999999956 ) ) ;
#20008 = ORIENTED_EDGE ( 'NONE', *, *, #15761, .F. ) ;
#20007 = FACE_OUTER_BOUND ( 'NONE', #11687, .T. ) ;
#20009 = ORIENTED_EDGE ( 'NONE', *, *, #14381, .T. ) ;
#20010 = DIRECTION ( 'NONE',  ( 0.000000000000000000, -1.000000000000000000, 0.000000000000000000 ) ) ;
#20011 = ORIENTED_EDGE ( 'NONE', *, *, #7865, .F. ) ;
#20012 = EDGE_CURVE ( 'NONE', #2636, #19518, #8758, .T. ) ;
#20013 = ORIENTED_EDGE ( 'NONE', *, *, #21664, .F. ) ;
#20014 = VERTEX_POINT ( 'NONE', #5416 ) ;
#20015 = DIRECTION ( 'NONE',  ( 0.000000000000000000, 0.000000000000000000, -1.000000000000000000 ) ) ;
#20016=STYLED_ITEM('',(#25907),#13271);
#20017 = CIRCLE ( 'NONE', #22113, 0.5000000000000003331 ) ;
#20018 = ORIENTED_EDGE ( 'NONE', *, *, #16538, .T. ) ;
#20019 = FACE_OUTER_BOUND ( 'NONE', #22923, .T. ) ;
#20020 = CARTESIAN_POINT ( 'NONE',  ( 3.756430356250003211, 25.29062499938548569, 6.831223922626973533 ) ) ;
#20021 = AXIS2_PLACEMENT_3D ( 'NONE', #4240, #6463, #12219 ) ;
#20022 = DIRECTION ( 'NONE',  ( 0.000000000000000000, 0.000000000000000000, 1.000000000000000000 ) ) ;
#20023 = DIRECTION ( 'NONE',  ( -0.2486898871648449971, 0.9685831611286336296, 0.000000000000000000 ) ) ;
#20024 = CARTESIAN_POINT ( 'NONE',  ( 22.36900861179109867, 17.05661385587227841, 6.831223922626973533 ) ) ;
#20025 = EDGE_CURVE ( 'NONE', #21478, #13240, #25788, .T. ) ;
#20026 = DIRECTION ( 'NONE',  ( -1.000000000000000000, 0.000000000000000000, 0.000000000000000000 ) ) ;
#20027 = DIRECTION ( 'NONE',  ( 0.000000000000000000, -1.000000000000000000, 0.000000000000000000 ) ) ;
#20028 = CIRCLE ( 'NONE', #834, 4.000000000000000000 ) ;
#20029 = CARTESIAN_POINT ( 'NONE',  ( -3.756430356249995661, -6.831223922626973533, 0.7781249993854825187 ) ) ;
#20030 = EDGE_CURVE ( 'NONE', #2880, #672, #19405, .T. ) ;
#20031 = CARTESIAN_POINT ( 'NONE',  ( 4.000000000000003553, 27.70000000000000284, 8.999999999999992895 ) ) ;
#20032 = CARTESIAN_POINT ( 'NONE',  ( -3.756430356249996105, 29.37812499938548427, 6.831223922626973533 ) ) ;
#20033 = CIRCLE ( 'NONE', #838, 0.5000000000000003331 ) ;
#20034 = EDGE_CURVE ( 'NONE', #2494, #1926, #13760, .T. ) ;
#20035 = FACE_OUTER_BOUND ( 'NONE', #17781, .T. ) ;
#20036 = CARTESIAN_POINT ( 'NONE',  ( 19.18020767368691182, 21.83640505164621004, 5.746835883940462963 ) ) ;
#20037 = LINE ( 'NONE', #25677, #1587 ) ;
#20038 = EDGE_LOOP ( 'NONE', ( #13687, #16382, #5210, #17248 ) ) ;
#20039 = ORIENTED_EDGE ( 'NONE', *, *, #14360, .T. ) ;
#20040 = CARTESIAN_POINT ( 'NONE',  ( 1.878215178125003382, 26.67812499938548854, 5.746835883940462963 ) ) ;
#20041 = ORIENTED_EDGE ( 'NONE', *, *, #9608, .F. ) ;
#20042 = DIRECTION ( 'NONE',  ( 0.000000000000000000, 0.000000000000000000, 1.000000000000000000 ) ) ;
#20043 = CARTESIAN_POINT ( 'NONE',  ( 1.878215178125000939, 26.07812499938548356, 12.25316411605952283 ) ) ;
#20044 = DIRECTION ( 'NONE',  ( 1.000000000000000000, 0.000000000000000000, 0.000000000000000000 ) ) ;
#20045 = CARTESIAN_POINT ( 'NONE',  ( -1.071796769724487230, 28.28259618943233988, 4.999999999999992006 ) ) ;
#20046 = ORIENTED_EDGE ( 'NONE', *, *, #10422, .T. ) ;
#20047 = CARTESIAN_POINT ( 'NONE',  ( -9.110428525061097460, -29.57785765677920509, 1.000000000000000000 ) ) ;
#20048 = VERTEX_POINT ( 'NONE', #11159 ) ;
#20049 = DIRECTION ( 'NONE',  ( 1.000000000000000000, 0.000000000000000000, 0.000000000000000000 ) ) ;
#20050 = CARTESIAN_POINT ( 'NONE',  ( 3.735045420075836212E-15, 27.95312499938548001, 4.662447845253954171 ) ) ;
#20051 = CARTESIAN_POINT ( 'NONE',  ( 4.000000000000001776, 29.01249999999999929, 11.30940107675849760 ) ) ;
#20052 = AXIS2_PLACEMENT_3D ( 'NONE', #2235, #1968, #10192 ) ;
#20053 = CIRCLE ( 'NONE', #14223, 8.000000000000000000 ) ;
#20054 = CARTESIAN_POINT ( 'NONE',  ( 0.000000000000000000, 0.000000000000000000, 18.19999999999999929 ) ) ;
#20055 = CARTESIAN_POINT ( 'NONE',  ( -9.110428525060477511, 29.57785765677940404, -6.500000000000000000 ) ) ;
#20056 = CARTESIAN_POINT ( 'NONE',  ( -3.999999999999996447, 29.23750000000000782, 6.690598923241487306 ) ) ;
#20057 = ADVANCED_FACE ( 'NONE', ( #23202 ), #8831, .F. ) ;
#20058 = CARTESIAN_POINT ( 'NONE',  ( -3.756430356249995661, 25.77812499938548640, 6.831223922626973533 ) ) ;
#20059 = EDGE_CURVE ( 'NONE', #21505, #6156, #4991, .T. ) ;
#20060 = CARTESIAN_POINT ( 'NONE',  ( 2.620986760973688460E-15, -13.61880215351699874, 1.181249998770967258 ) ) ;
#20061 = AXIS2_PLACEMENT_3D ( 'NONE', #6452, #14554, #12208 ) ;
#20062 = CARTESIAN_POINT ( 'NONE',  ( 0.000000000000000000, -31.10000000000000142, -6.500000000000000000 ) ) ;
#20063 = LINE ( 'NONE', #10130, #24583 ) ;
#20064 = PRODUCT ( 'spindle', 'spindle', '', ( #1252 ) ) ;
#20065 = DIRECTION ( 'NONE',  ( -0.000000000000000000, -0.000000000000000000, 1.000000000000000000 ) ) ;
#20066 = CARTESIAN_POINT ( 'NONE',  ( 17.87326343783925253, -25.45105997952931176, -2.750000000000000000 ) ) ;
#20067 = ADVANCED_FACE ( 'NONE', ( #20851 ), #15353, .T. ) ;
#20068 = FACE_OUTER_BOUND ( 'NONE', #23053, .T. ) ;
#20069 = CIRCLE ( 'NONE', #8811, 0.5000000000000005551 ) ;
#20070 = CARTESIAN_POINT ( 'NONE',  ( -1.878215178125000939, -25.51562499938548356, 12.25316411605952283 ) ) ;
#20071 = CIRCLE ( 'NONE', #9646, 0.5000000000000006661 ) ;
#20072 = FACE_OUTER_BOUND ( 'NONE', #2748, .T. ) ;
#20073 = EDGE_LOOP ( 'NONE', ( #4546, #25496, #817, #23437 ) ) ;
#20074 = CARTESIAN_POINT ( 'NONE',  ( -3.999999999999996003, 28.28124999877096712, 6.690598923241487306 ) ) ;
#20076 = VERTEX_POINT ( 'NONE', #9214 ) ;
#20075 = CARTESIAN_POINT ( 'NONE',  ( -3.756430356249994329, 26.79062499938548925, 6.831223922626973533 ) ) ;
#20077 = CIRCLE ( 'NONE', #22591, 4.000000000000000000 ) ;
#20078 = CARTESIAN_POINT ( 'NONE',  ( 3.756430356250002323, 28.36562499938548854, 11.16877607737301403 ) ) ;
#20079 = CIRCLE ( 'NONE', #25526, 26.00000000000000711 ) ;
#20080 = LINE ( 'NONE', #219, #8817 ) ;
#20081 = DIRECTION ( 'NONE',  ( 1.000000000000000000, 0.000000000000000000, 0.000000000000000000 ) ) ;
#20082 = ORIENTED_EDGE ( 'NONE', *, *, #25288, .T. ) ;
#20083 = ORIENTED_EDGE ( 'NONE', *, *, #19066, .F. ) ;
#20084 = CARTESIAN_POINT ( 'NONE',  ( 1.878215178124998497, -25.55312499938548854, 12.25316411605951927 ) ) ;
#20085 = CARTESIAN_POINT ( 'NONE',  ( -2.003086131649545506E-15, 26.82812499938549067, 13.33755215474602984 ) ) ;
#20086 = CARTESIAN_POINT ( 'NONE',  ( 22.08382865906333947, 16.42697440957088872, 6.690598923241489970 ) ) ;
#20087 = CARTESIAN_POINT ( 'NONE',  ( -1.878215178124995832, -5.746835883940462963, 2.540624999385482141 ) ) ;
#20088 = AXIS2_PLACEMENT_3D ( 'NONE', #8604, #14880, #10679 ) ;
#20089 = VECTOR ( 'NONE', #20414, 999.9999999999998863 ) ;
#20090 = SURFACE_STYLE_USAGE ( .BOTH. , #4139 ) ;
#20091 = EDGE_CURVE ( 'NONE', #21352, #19826, #19019, .T. ) ;
#20092 = CARTESIAN_POINT ( 'NONE',  ( 0.5000000000000000000, -0.8660254037844387076, 19.50000000000000000 ) ) ;
#20093 = AXIS2_PLACEMENT_3D ( 'NONE', #7943, #15930, #23761 ) ;
#20094 = EDGE_CURVE ( 'NONE', #2304, #12209, #24910, .T. ) ;
#20095 = CARTESIAN_POINT ( 'NONE',  ( 30.54913349766219710, -5.827558883616158703, -6.500000000000000000 ) ) ;
#20096 = CARTESIAN_POINT ( 'NONE',  ( 4.000000000000005329, 29.44374999877097210, 8.999999999999992895 ) ) ;
#20097 = CARTESIAN_POINT ( 'NONE',  ( 0.000000000000000000, 0.000000000000000000, -6.500000000000000000 ) ) ;
#20098 = DIRECTION ( 'NONE',  ( 0.3681245526846732008, -0.9297764858882532346, 0.000000000000000000 ) ) ;
#20099 = DIRECTION ( 'NONE',  ( 1.000000000000000000, 0.000000000000000000, 0.000000000000000000 ) ) ;
#20100 = CARTESIAN_POINT ( 'NONE',  ( 17.19595303411133713, 22.85280728360364577, 8.999999999999992895 ) ) ;
#20101 = ORIENTED_EDGE ( 'NONE', *, *, #23227, .F. ) ;
#20102 = FACE_OUTER_BOUND ( 'NONE', #25621, .T. ) ;
#20103 = DIRECTION ( 'NONE',  ( 0.000000000000000000, 1.000000000000000000, -0.000000000000000000 ) ) ;
#20104 = CARTESIAN_POINT ( 'NONE',  ( 3.756430356250004099, 25.62812499938548072, 6.831223922626973533 ) ) ;
#20105 = CARTESIAN_POINT ( 'NONE',  ( -30.85476721088030061, -3.897863563849544466, -6.500000000000000000 ) ) ;
#20106 = AXIS2_PLACEMENT_3D ( 'NONE', #13953, #6454, #13683 ) ;
#20107 = CARTESIAN_POINT ( 'NONE',  ( -1.999999999999994893, 29.14374999877097139, 5.535898384862237620 ) ) ;
#20108 = CARTESIAN_POINT ( 'NONE',  ( 4.000000000000003553, -8.999999999999992895, 1.350000000000000533 ) ) ;
#20109 = VERTEX_POINT ( 'NONE', #21112 ) ;
#20110 = CYLINDRICAL_SURFACE ( 'NONE', #23867, 31.10000000000000142 ) ;
#20111 = CARTESIAN_POINT ( 'NONE',  ( 2.000000000000003997, 26.36874999877096926, 5.535898384862238508 ) ) ;
#20112 = CARTESIAN_POINT ( 'NONE',  ( 1.878215178124995832, -25.29062499938548569, 5.746835883940462963 ) ) ;
#20114 = EDGE_LOOP ( 'NONE', ( #9473, #23947, #1272, #24004 ) ) ;
#20113 = CYLINDRICAL_SURFACE ( 'NONE', #2473, 4.000000000000000000 ) ;
#20115 = CIRCLE ( 'NONE', #22633, 0.5000000000000003331 ) ;
#20116 = ADVANCED_FACE ( 'NONE', ( #18902 ), #7376, .T. ) ;
#20117 = ORIENTED_EDGE ( 'NONE', *, *, #24489, .F. ) ;
#20118 = ORIENTED_EDGE ( 'NONE', *, *, #1898, .T. ) ;
#20119 = ORIENTED_EDGE ( 'NONE', *, *, #16370, .F. ) ;
#20120 = CARTESIAN_POINT ( 'NONE',  ( -5.327558883616270613, -30.54913349766217934, 1.000000000000000000 ) ) ;
#20122 = CARTESIAN_POINT ( 'NONE',  ( -3.756430356249996105, 26.34062499938548285, 6.831223922626973533 ) ) ;
#20121 = CIRCLE ( 'NONE', #10505, 31.10000000000000142 ) ;
#20123 = CARTESIAN_POINT ( 'NONE',  ( -1.999999999999998224, 26.59374999877096712, 12.46410161513774639 ) ) ;
#20124 = CARTESIAN_POINT ( 'NONE',  ( -2.003086131649545506E-15, 26.82812499938549067, 13.33755215474602984 ) ) ;
#20125 = PLANE ( 'NONE',  #16788 ) ;
#20126 = CARTESIAN_POINT ( 'NONE',  ( -3.999999999999997335, -11.30940107675849404, 3.356249998770967746 ) ) ;
#20127 = CIRCLE ( 'NONE', #18894, 31.10000000000000142 ) ;
#20128 = CARTESIAN_POINT ( 'NONE',  ( -3.756430356249995661, 29.49062499938548498, 6.831223922626973533 ) ) ;
#20129 = CIRCLE ( 'NONE', #22229, 0.4999999999999999445 ) ;
#20130 = DIRECTION ( 'NONE',  ( -0.9980267284282710039, 0.06279051952932233893, 0.000000000000000000 ) ) ;
#20131 = CARTESIAN_POINT ( 'NONE',  ( 20.92219106202050583, 23.01025686871638598, 1.000000000000000000 ) ) ;
#20132 = CARTESIAN_POINT ( 'NONE',  ( 2.672651547586948120E-15, 26.82812499938548356, 13.33755215474603162 ) ) ;
#20133 = DIRECTION ( 'NONE',  ( 0.000000000000000000, 0.000000000000000000, -1.000000000000000000 ) ) ;
#20134 = CARTESIAN_POINT ( 'NONE',  ( 0.7500000000000000000, -2.999999999999999556, 17.69999999999999929 ) ) ;
#20135 = DIRECTION ( 'NONE',  ( 0.000000000000000000, 0.000000000000000000, 1.000000000000000000 ) ) ;
#20136 = CARTESIAN_POINT ( 'NONE',  ( 3.756430356249996994, -25.47812499938548569, 8.999999999999992895 ) ) ;
#20137 = AXIS2_PLACEMENT_3D ( 'NONE', #8211, #10165, #15937 ) ;
#20138 = CARTESIAN_POINT ( 'NONE',  ( -11.44867358849309547, 28.91604871112477326, 1.000000000000000000 ) ) ;
#20139 = CARTESIAN_POINT ( 'NONE',  ( 0.000000000000000000, 0.000000000000000000, -6.500000000000000000 ) ) ;
#20140 = CARTESIAN_POINT ( 'NONE',  ( -1.998723687422152831E-12, 39.00000000001113420, 14.49999999998978240 ) ) ;
#20141 = CARTESIAN_POINT ( 'NONE',  ( 3.999999999999995559, -26.03124999877097068, 6.690598923241487306 ) ) ;
#20142 = EDGE_CURVE ( 'NONE', #22705, #21476, #6230, .T. ) ;
#20143 = ORIENTED_EDGE ( 'NONE', *, *, #23166, .F. ) ;
#20144 = CARTESIAN_POINT ( 'NONE',  ( 1.071796769724487675, 28.69240381056766509, 4.999999999999988454 ) ) ;
#20146 = ORIENTED_EDGE ( 'NONE', *, *, #19020, .F. ) ;
#20145 = FACE_OUTER_BOUND ( 'NONE', #12201, .T. ) ;
#20147 =( BOUNDED_CURVE ( )  B_SPLINE_CURVE ( 2, ( #23807, #1973, #15, #10197, #663, #10072, #24065, #20263, #8632 ),
 .UNSPECIFIED., .F., .F. ) 
 B_SPLINE_CURVE_WITH_KNOTS ( ( 3, 2, 2, 2, 3 ),
 ( 0.2250000000000000056, 0.2333333333333333370, 0.2500000000000000000, 0.2666666666666666630, 0.2750000000000000222 ),
 .UNSPECIFIED. ) 
 CURVE ( )  GEOMETRIC_REPRESENTATION_ITEM ( )  RATIONAL_B_SPLINE_CURVE ( ( 0.9330127018922194093, 0.9330127018922194093, 1.000000000000000000, 0.8660254037844387076, 1.000000000000000000, 0.8660254037844387076, 1.000000000000000000, 0.9330127018922191873, 0.9330127018922194093 ) ) 
 REPRESENTATION_ITEM ( '' )  );
#20148 = CIRCLE ( 'NONE', #24339, 0.4999999999999998335 ) ;
#20149 = VERTEX_POINT ( 'NONE', #5934 ) ;
#20150 = VERTEX_POINT ( 'NONE', #15746 ) ;
#20151 = VERTEX_POINT ( 'NONE', #3581 ) ;
#20152 = ORIENTED_EDGE ( 'NONE', *, *, #3035, .T. ) ;
#20153 = AXIS2_PLACEMENT_3D ( 'NONE', #9177, #11257, #1342 ) ;
#20154 = ORIENTED_EDGE ( 'NONE', *, *, #3296, .F. ) ;
#20155 = CARTESIAN_POINT ( 'NONE',  ( 4.000000000000003553, 28.60000000000000142, 8.999999999999992895 ) ) ;
#20156 = CARTESIAN_POINT ( 'NONE',  ( 2.672651547586948120E-15, 26.49062499938548498, 13.33755215474603162 ) ) ;
#20157 = AXIS2_PLACEMENT_3D ( 'NONE', #6550, #5495, #7208 ) ;
#20158 = CARTESIAN_POINT ( 'NONE',  ( 1.878215178125004048, -5.746835883940462963, 3.028124999385484184 ) ) ;
#20159 = CARTESIAN_POINT ( 'NONE',  ( 30.10000000000000142, 0.000000000000000000, 0.000000000000000000 ) ) ;
#20160 = CARTESIAN_POINT ( 'NONE',  ( 17.61573392031167273, 20.27193129827097806, 12.25316411605951927 ) ) ;
#20161 = LINE ( 'NONE', #10477, #7972 ) ;
#20162 = VECTOR ( 'NONE', #17664, 1000.000000000000000 ) ;
#20163 = CARTESIAN_POINT ( 'NONE',  ( 1.878215178125004048, -5.746835883940462963, 2.465624999385483740 ) ) ;
#20164 = EDGE_CURVE ( 'NONE', #17619, #13787, #4087, .T. ) ;
#20165 = CARTESIAN_POINT ( 'NONE',  ( 0.000000000000000000, 0.000000000000000000, 17.00000000000000000 ) ) ;
#20166 = CARTESIAN_POINT ( 'NONE',  ( -3.756430356249996994, 28.51562499938548356, 8.999999999999992895 ) ) ;
#20167 = CARTESIAN_POINT ( 'NONE',  ( 2.000000000000000888, -12.46410161513774817, 3.525000000000000355 ) ) ;
#20168 = DIRECTION ( 'NONE',  ( 1.000000000000000000, 0.000000000000000000, 0.000000000000000000 ) ) ;
#20169 = CYLINDRICAL_SURFACE ( 'NONE', #8687, 0.4999999999999995559 ) ;
#20170 = VERTEX_POINT ( 'NONE', #1619 ) ;
#20171 = ORIENTED_EDGE ( 'NONE', *, *, #9208, .T. ) ;
#20172 = CARTESIAN_POINT ( 'NONE',  ( 0.000000000000000000, 27.84062499938548996, 13.33755215474602984 ) ) ;
#20173 = EDGE_CURVE ( 'NONE', #19025, #3732, #6080, .T. ) ;
#20174 = EDGE_LOOP ( 'NONE', ( #333, #5559 ) ) ;
#20175 = DIRECTION ( 'NONE',  ( -0.9685831611286283005, 0.2486898871648657861, 0.000000000000000000 ) ) ;
#20176 = ORIENTED_EDGE ( 'NONE', *, *, #2762, .F. ) ;
#20177 = ADVANCED_FACE ( 'NONE', ( #5672 ), #21618, .F. ) ;
#20178 = ORIENTED_EDGE ( 'NONE', *, *, #422, .T. ) ;
#20179 = CONICAL_SURFACE ( 'NONE', #11004, 5.000000000000000888, 0.7853981633974445042 ) ;
#20180 = CARTESIAN_POINT ( 'NONE',  ( -3.999999999999999112, 26.10624999877097707, 11.30940107675849404 ) ) ;
#20181 = ORIENTED_EDGE ( 'NONE', *, *, #16240, .T. ) ;
#20182 = EDGE_CURVE ( 'NONE', #16757, #11943, #9996, .T. ) ;
#20183 = DIRECTION ( 'NONE',  ( 0.000000000000000000, 0.000000000000000000, -1.000000000000000000 ) ) ;
#20184 = CARTESIAN_POINT ( 'NONE',  ( -3.756430356249997882, 28.10312499938548569, 11.16877607737301226 ) ) ;
#20185 = CARTESIAN_POINT ( 'NONE',  ( 0.5000000000000000000, 0.000000000000000000, 20.00000000000000000 ) ) ;
#20186 = DIRECTION ( 'NONE',  ( 0.000000000000000000, 1.000000000000000000, 0.000000000000000000 ) ) ;
#20187 = CYLINDRICAL_SURFACE ( 'NONE', #403, 31.10000000000000142 ) ;
#20188 = CARTESIAN_POINT ( 'NONE',  ( 0.000000000000000000, 28.48750000000000426, 13.61880215351699874 ) ) ;
#20189 = PRESENTATION_LAYER_ASSIGNMENT (  '', '', ( #8922 ) ) ;
#20190 = CARTESIAN_POINT ( 'NONE',  ( 1.878215178125000939, 25.51562499938548356, 12.25316411605952283 ) ) ;
#20191 = CARTESIAN_POINT ( 'NONE',  ( -1.071796769724485454, 26.21740381056766367, 12.99999999999999467 ) ) ;
#20192 = AXIS2_PLACEMENT_3D ( 'NONE', #21126, #23215, #5429 ) ;
#20193 = LINE ( 'NONE', #3422, #13316 ) ;
#20194 = CARTESIAN_POINT ( 'NONE',  ( 19.66640735175089105, 19.66640735175081289, 4.999999999999992006 ) ) ;
#20195 = PLANE ( 'NONE',  #18046 ) ;
#20196 = CARTESIAN_POINT ( 'NONE',  ( 3.369928719974892281E-15, 25.11250000000000426, 4.999999999999992006 ) ) ;
#20197 = CARTESIAN_POINT ( 'NONE',  ( -3.756430356250003655, -26.04062499938548569, 8.999999999999992895 ) ) ;
#20198 = FACE_OUTER_BOUND ( 'NONE', #17778, .T. ) ;
#20199 = EDGE_LOOP ( 'NONE', ( #2338, #18874, #25809, #7289 ) ) ;
#20200 = CARTESIAN_POINT ( 'NONE',  ( -3.999999999999996003, 27.38124999877096855, 6.690598923241487306 ) ) ;
#20201 = LINE ( 'NONE', #20326, #19620 ) ;
#20203 = EDGE_LOOP ( 'NONE', ( #9444, #1733, #5973, #22771 ) ) ;
#20202 = CARTESIAN_POINT ( 'NONE',  ( 2.003086131649545506E-15, 26.94062499938549138, 13.33755215474603162 ) ) ;
#20204 = ORIENTED_EDGE ( 'NONE', *, *, #23591, .T. ) ;
#20205 = CARTESIAN_POINT ( 'NONE',  ( 1.878215178125000939, 27.42812499938548498, 12.25316411605952283 ) ) ;
#20206 = MECHANICAL_DESIGN_GEOMETRIC_PRESENTATION_REPRESENTATION (  '', ( #3510 ), #595 ) ;
#20207 = DIRECTION ( 'NONE',  ( 0.000000000000000000, 1.000000000000000000, -0.000000000000000000 ) ) ;
#20208 = CARTESIAN_POINT ( 'NONE',  ( 0.000000000000000000, 0.000000000000000000, -6.500000000000000000 ) ) ;
#20209 = ORIENTED_EDGE ( 'NONE', *, *, #6190, .T. ) ;
#20210 = VERTEX_POINT ( 'NONE', #15625 ) ;
#20211 = EDGE_CURVE ( 'NONE', #10774, #6810, #21694, .T. ) ;
#20212 = CARTESIAN_POINT ( 'NONE',  ( -3.756430356250003655, -26.60312499938548569, 8.999999999999992895 ) ) ;
#20213 = CARTESIAN_POINT ( 'NONE',  ( 8.012344526598182026E-15, 27.05312499938548854, 4.662447845253954171 ) ) ;
#20214 = CARTESIAN_POINT ( 'NONE',  ( 19.14933551713917126, 19.14933551713910376, 12.99999999999999289 ) ) ;
#20215 = ADVANCED_FACE ( 'NONE', ( #17446 ), #23593, .T. ) ;
#20216 = CARTESIAN_POINT ( 'NONE',  ( 3.756430356250002323, -11.16877607737301403, 3.253124999385482941 ) ) ;
#20217 = EDGE_CURVE ( 'NONE', #12173, #19269, #13918, .T. ) ;
#20218 = CARTESIAN_POINT ( 'NONE',  ( 3.469446951953614189E-15, 30.00000000000000355, 8.999999999999992895 ) ) ;
#20219 = DIRECTION ( 'NONE',  ( 0.000000000000000000, 0.000000000000000000, -1.000000000000000000 ) ) ;
#20220 = CARTESIAN_POINT ( 'NONE',  ( 0.7500000000000000000, -1.299038105676658450, 17.69999999999999929 ) ) ;
#20221 = CARTESIAN_POINT ( 'NONE',  ( 0.000000000000000000, 0.000000000000000000, 1.000000000000000000 ) ) ;
#20222 = AXIS2_PLACEMENT_3D ( 'NONE', #10662, #24803, #1004 ) ;
#20223 = ADVANCED_FACE ( 'NONE', ( #6061 ), #19657, .F. ) ;
#20224 = CARTESIAN_POINT ( 'NONE',  ( 8.831537335106614961E-15, 26.63124999877096855, 12.99999999999999112 ) ) ;
#20225 = DIRECTION ( 'NONE',  ( -0.000000000000000000, -0.000000000000000000, -1.000000000000000000 ) ) ;
#20226 = CARTESIAN_POINT ( 'NONE',  ( 16.20808571844850121, 21.52048047436717937, 6.831223922626973533 ) ) ;
#20227 = CARTESIAN_POINT ( 'NONE',  ( 22.69370825783673951, 17.03685400834428521, 8.999999999999992895 ) ) ;
#20228 = ORIENTED_EDGE ( 'NONE', *, *, #9005, .F. ) ;
#20229 = CARTESIAN_POINT ( 'NONE',  ( 1.999999999999995781, -26.95000000000000284, 5.535898384862237620 ) ) ;
#20230 = DIRECTION ( 'NONE',  ( -0.000000000000000000, -0.000000000000000000, 1.000000000000000000 ) ) ;
#20231 = CARTESIAN_POINT ( 'NONE',  ( 3.756430356250003655, 29.30312499938548498, 8.999999999999992895 ) ) ;
#20233 = ORIENTED_EDGE ( 'NONE', *, *, #15211, .F. ) ;
#20232 = CARTESIAN_POINT ( 'NONE',  ( -3.974007292349814424, 29.73566758725665338, 9.525109153848150711 ) ) ;
#20234 = CARTESIAN_POINT ( 'NONE',  ( 19.47643616943617317, 16.82023879147673284, 5.746835883940462963 ) ) ;
#20235 = CARTESIAN_POINT ( 'NONE',  ( 1.071796769724487230, -27.83259618943233704, 4.999999999999992006 ) ) ;
#20236 = ORIENTED_EDGE ( 'NONE', *, *, #11708, .T. ) ;
#20237 = CARTESIAN_POINT ( 'NONE',  ( -1.999999999999998224, 25.69374999877097210, 12.46410161513774639 ) ) ;
#20238 = CARTESIAN_POINT ( 'NONE',  ( -2.672651547586948120E-15, -25.47812499938548569, 13.33755215474602984 ) ) ;
#20240 = ORIENTED_EDGE ( 'NONE', *, *, #25688, .T. ) ;
#20239 = CARTESIAN_POINT ( 'NONE',  ( 3.253724281355068545E-15, 25.50624999877097210, 4.999999999999992006 ) ) ;
#20241 = VERTEX_POINT ( 'NONE', #8030 ) ;
#20242 = EDGE_CURVE ( 'NONE', #11825, #5668, #7245, .T. ) ;
#20243 = VECTOR ( 'NONE', #7771, 1000.000000000000000 ) ;
#20244 = ORIENTED_EDGE ( 'NONE', *, *, #1611, .T. ) ;
#20245 = ORIENTED_EDGE ( 'NONE', *, *, #11594, .T. ) ;
#20246 = DIRECTION ( 'NONE',  ( 0.000000000000000000, -0.000000000000000000, 1.000000000000000000 ) ) ;
#20247 = CARTESIAN_POINT ( 'NONE',  ( -3.756430356249994773, 26.37812499938548783, 8.999999999999992895 ) ) ;
#20248 = EDGE_CURVE ( 'NONE', #4968, #2690, #14599, .T. ) ;
#20249 = DIRECTION ( 'NONE',  ( 0.000000000000000000, -0.000000000000000000, 1.000000000000000000 ) ) ;
#20250 = CARTESIAN_POINT ( 'NONE',  ( 1.878215178125000939, -12.25316411605952283, 4.565624999385481608 ) ) ;
#20251 = CARTESIAN_POINT ( 'NONE',  ( 3.756430356250002323, -11.16877607737301226, 0.6656249993854835845 ) ) ;
#20252 = FILL_AREA_STYLE ('',( #10059 ) ) ;
#20253 = CARTESIAN_POINT ( 'NONE',  ( 3.735045420075836212E-15, 27.05312499938548498, 4.662447845253954171 ) ) ;
#20254 = EDGE_CURVE ( 'NONE', #18582, #25179, #9852, .T. ) ;
#20255 = DIRECTION ( 'NONE',  ( 1.000000000000000000, 0.000000000000000000, -0.000000000000000000 ) ) ;
#20256 = DIRECTION ( 'NONE',  ( 0.000000000000000000, 0.000000000000000000, 1.000000000000000000 ) ) ;
#20257 = CARTESIAN_POINT ( 'NONE',  ( -3.756430356249996994, 26.71562499938548285, 8.999999999999992895 ) ) ;
#20258 = DIRECTION ( 'NONE',  ( 0.000000000000000000, 0.000000000000000000, 1.000000000000000000 ) ) ;
#20259 = DIRECTION ( 'NONE',  ( 0.000000000000000000, 1.000000000000000000, -0.000000000000000000 ) ) ;
#20260 = CARTESIAN_POINT ( 'NONE',  ( 16.68772003600256326, 19.51614716074868028, 5.535898384862237620 ) ) ;
#20261 = CARTESIAN_POINT ( 'NONE',  ( 3.999999999999996003, -28.73124999877096641, 6.690598923241487306 ) ) ;
#20262 = CARTESIAN_POINT ( 'NONE',  ( 9.296355089585910693E-16, 26.18124999877097281, 12.99999999999999289 ) ) ;
#20263 = CARTESIAN_POINT ( 'NONE',  ( 1.071796769724485454, -26.21740381056766367, 12.99999999999999467 ) ) ;
#20264 = CARTESIAN_POINT ( 'NONE',  ( 2.620986760973688460E-15, -13.61880215351699874, 1.687500000000000000 ) ) ;
#20265 = CARTESIAN_POINT ( 'NONE',  ( 1.626862140677534194E-14, 28.03750000000000497, 12.99999999999999289 ) ) ;
#20266 = VERTEX_POINT ( 'NONE', #10349 ) ;
#20267 = CARTESIAN_POINT ( 'NONE',  ( 2.000000000000000000, 27.56874999877097210, 12.46410161513774817 ) ) ;
#20269 = ORIENTED_EDGE ( 'NONE', *, *, #17042, .F. ) ;
#20268 = DIRECTION ( 'NONE',  ( -2.891205793294678326E-16, -1.000000000000000000, 0.000000000000000000 ) ) ;
#20270 = ORIENTED_EDGE ( 'NONE', *, *, #18989, .F. ) ;
#20271 = ORIENTED_EDGE ( 'NONE', *, *, #10247, .T. ) ;
#20272 = ORIENTED_EDGE ( 'NONE', *, *, #23591, .F. ) ;
#20273 = EDGE_LOOP ( 'NONE', ( #21281, #23052, #20900, #25719 ) ) ;
#20274 = ORIENTED_EDGE ( 'NONE', *, *, #1250, .F. ) ;
#20275 = DIRECTION ( 'NONE',  ( 1.000000000000000000, 0.000000000000000000, 0.000000000000000000 ) ) ;
#20276 = EDGE_CURVE ( 'NONE', #25560, #23884, #24233, .T. ) ;
#20277 = VERTEX_POINT ( 'NONE', #14316 ) ;
#20278 = AXIS2_PLACEMENT_3D ( 'NONE', #4484, #315, #14050 ) ;
#20279 = CARTESIAN_POINT ( 'NONE',  ( 23.26836714124207361, 18.93629030671969460, 11.57226653943513028 ) ) ;
#20280 = CARTESIAN_POINT ( 'NONE',  ( 1.878215178125000939, 25.62812499938548783, 12.25316411605952283 ) ) ;
#20281 = EDGE_CURVE ( 'NONE', #23846, #19738, #447, .T. ) ;
#20282 = CARTESIAN_POINT ( 'NONE',  ( -1.878215178124998497, -12.25316411605951927, 3.253124999385483829 ) ) ;
#20283 = CARTESIAN_POINT ( 'NONE',  ( 0.000000000000000000, 0.000000000000000000, 1.000000000000000000 ) ) ;
#20284 = CARTESIAN_POINT ( 'NONE',  ( 21.99777755166815751, 16.68538279574934435, 11.16877607737301226 ) ) ;
#20285 =( BOUNDED_CURVE ( )  B_SPLINE_CURVE ( 2, ( #4221, #24225, #6312, #14307, #7566, #13704, #3244, #13325, #15417 ),
 .UNSPECIFIED., .F., .F. ) 
 B_SPLINE_CURVE_WITH_KNOTS ( ( 3, 2, 2, 2, 3 ),
 ( 0.5250000000000000222, 0.5333333333333333259, 0.5500000000000000444, 0.5666666666666666519, 0.5750000000000000666 ),
 .UNSPECIFIED. ) 
 CURVE ( )  GEOMETRIC_REPRESENTATION_ITEM ( )  RATIONAL_B_SPLINE_CURVE ( ( 0.9330127018922194093, 0.9330127018922194093, 1.000000000000000000, 0.8660254037844387076, 1.000000000000000000, 0.8660254037844387076, 1.000000000000000000, 0.9330127018922189652, 0.9330127018922194093 ) ) 
 REPRESENTATION_ITEM ( '' )  );
#20286 = CARTESIAN_POINT ( 'NONE',  ( 18.91510639674018890, 21.74353352148630236, 5.535898384862237620 ) ) ;
#20287 = LINE ( 'NONE', #18336, #14215 ) ;
#20288 = ITEM_DEFINED_TRANSFORMATION ( 'NONE', 'NONE', #20222,  #21036 ) ;
#20289 = CARTESIAN_POINT ( 'NONE',  ( -1.878215178124995832, -5.746835883940462963, 2.090624999385483296 ) ) ;
#20290 = DIRECTION ( 'NONE',  ( 0.000000000000000000, 0.000000000000000000, 1.000000000000000000 ) ) ;
#20291 = CARTESIAN_POINT ( 'NONE',  ( 2.672651547586948120E-15, 29.52812499938548285, 13.33755215474603162 ) ) ;
#20292 =( BOUNDED_CURVE ( )  B_SPLINE_CURVE ( 2, ( #3612, #19819, #11581, #19554, #19315, #3493, #9763, #7672, #23623, #9633, #11719, #13442, #5701, #1410, #13680, #17364, #17867, #17611, #5829, #25588, #21653, #7409, #25839, #17742, #13816, #7922, #15909, #5967, #21412, #2178, #10139, #16557, #18143, #12100, #12362, #8064, #4121, #20457, #3999, #18003, #14203, #20075, #10009, #22305, #216, #20202, #6088, #11966, #18522, #4382, #10525, #92, #8186, #12235, #2041, #16046, #19937, #16164, #24127, #609, #6350, #8576, #16296, #24008, #24516, #6213, #2556, #4261, #13950, #14072, #21918, #8448, #22176, #2303, #8310, #10259, #479, #18253, #14463, #22038, #336, #24263, #14343, #20327, #2417, #10379, #18379, #16437, #24401, #6477, #22426, #4506, #12484, #16944, #1106, #2944, #6869, #14973, #20999, #18642, #6989, #7127, #12758, #3076, #22704, #2808, #6599, #6735, #8969, #4901, #10910, #22951, #4784, #25039, #20730, #20601, #24913, #10772, #11042, #14585, #4648 ),
 .UNSPECIFIED., .F., .F. ) 
 B_SPLINE_CURVE_WITH_KNOTS ( ( 3, 2, 2, 2, 2, 2, 2, 2, 2, 2, 2, 2, 2, 2, 2, 2, 2, 2, 2, 2, 2, 2, 2, 2, 2, 2, 2, 2, 2, 2, 2, 2, 2, 2, 2, 2, 2, 2, 2, 2, 2, 2, 2, 2, 2, 2, 2, 2, 2, 2, 2, 2, 2, 2, 2, 2, 2, 2, 2, 2, 3 ),
 ( 0.000000000000000000, 0.01666666666666666644, 0.03333333333333333287, 0.05000000000000000278, 0.06666666666666666574, 0.08333333333333332871, 0.1000000000000000056, 0.1166666666666666685, 0.1333333333333333315, 0.1499999999999999944, 0.1666666666666666574, 0.1833333333333333204, 0.2000000000000000111, 0.2166666666666666741, 0.2333333333333333370, 0.2500000000000000000, 0.2666666666666666630, 0.2833333333333333259, 0.2999999999999999889, 0.3166666666666666519, 0.3333333333333333148, 0.3499999999999999778, 0.3666666666666666408, 0.3833333333333333592, 0.4000000000000000222, 0.4166666666666666852, 0.4333333333333333481, 0.4500000000000000111, 0.4666666666666666741, 0.4833333333333333370, 0.5000000000000000000, 0.5166666666666667185, 0.5333333333333333259, 0.5500000000000000444, 0.5666666666666666519, 0.5833333333333333703, 0.5999999999999999778, 0.6166666666666666963, 0.6333333333333333037, 0.6500000000000000222, 0.6666666666666666297, 0.6833333333333333481, 0.6999999999999999556, 0.7166666666666666741, 0.7333333333333332815, 0.7500000000000000000, 0.7666666666666667185, 0.7833333333333333259, 0.8000000000000000444, 0.8166666666666666519, 0.8333333333333333703, 0.8499999999999999778, 0.8666666666666666963, 0.8833333333333333037, 0.9000000000000000222, 0.9166666666666666297, 0.9333333333333333481, 0.9499999999999999556, 0.9666666666666666741, 0.9833333333333332815, 1.000000000000000000 ),
 .UNSPECIFIED. ) 
 CURVE ( )  GEOMETRIC_REPRESENTATION_ITEM ( )  RATIONAL_B_SPLINE_CURVE ( ( 1.000000000000000000, 0.8660254037844387076, 1.000000000000000000, 0.8660254037844387076, 1.000000000000000000, 0.8660254037844387076, 1.000000000000000000, 0.8660254037844387076, 1.000000000000000000, 0.8660254037844387076, 1.000000000000000000, 0.8660254037844387076, 1.000000000000000000, 0.8660254037844387076, 1.000000000000000000, 0.8660254037844387076, 1.000000000000000000, 0.8660254037844387076, 1.000000000000000000, 0.8660254037844387076, 1.000000000000000000, 0.8660254037844387076, 1.000000000000000000, 0.8660254037844387076, 1.000000000000000000, 0.8660254037844387076, 1.000000000000000000, 0.8660254037844387076, 1.000000000000000000, 0.8660254037844387076, 1.000000000000000000, 0.8660254037844387076, 1.000000000000000000, 0.8660254037844387076, 1.000000000000000000, 0.8660254037844387076, 1.000000000000000000, 0.8660254037844387076, 1.000000000000000000, 0.8660254037844387076, 1.000000000000000000, 0.8660254037844387076, 1.000000000000000000, 0.8660254037844387076, 1.000000000000000000, 0.8660254037844387076, 1.000000000000000000, 0.8660254037844387076, 1.000000000000000000, 0.8660254037844387076, 1.000000000000000000, 0.8660254037844387076, 1.000000000000000000, 0.8660254037844387076, 1.000000000000000000, 0.8660254037844387076, 1.000000000000000000, 0.8660254037844387076, 1.000000000000000000, 0.8660254037844387076, 1.000000000000000000, 0.8660254037844387076, 1.000000000000000000, 0.8660254037844387076, 1.000000000000000000, 0.8660254037844387076, 1.000000000000000000, 0.8660254037844387076, 1.000000000000000000, 0.8660254037844387076, 1.000000000000000000, 0.8660254037844387076, 1.000000000000000000, 0.8660254037844387076, 1.000000000000000000, 0.8660254037844387076, 1.000000000000000000, 0.8660254037844387076, 1.000000000000000000, 0.8660254037844387076, 1.000000000000000000, 0.8660254037844387076, 1.000000000000000000, 0.8660254037844387076, 1.000000000000000000, 0.8660254037844387076, 1.000000000000000000, 0.8660254037844387076, 1.000000000000000000, 0.8660254037844387076, 1.000000000000000000, 0.8660254037844387076, 1.000000000000000000, 0.8660254037844387076, 1.000000000000000000, 0.8660254037844387076, 1.000000000000000000, 0.8660254037844387076, 1.000000000000000000, 0.8660254037844387076, 1.000000000000000000, 0.8660254037844387076, 1.000000000000000000, 0.8660254037844387076, 1.000000000000000000, 0.8660254037844387076, 1.000000000000000000, 0.8660254037844387076, 1.000000000000000000, 0.8660254037844387076, 1.000000000000000000, 0.8660254037844387076, 1.000000000000000000, 0.8660254037844387076, 1.000000000000000000, 0.8660254037844387076, 1.000000000000000000, 0.8660254037844387076, 1.000000000000000000, 0.8660254037844387076, 1.000000000000000000 ) ) 
 REPRESENTATION_ITEM ( '' )  );
#20293 = CARTESIAN_POINT ( 'NONE',  ( 1.878215178125000939, -12.25316411605952283, 2.428124999385484539 ) ) ;
#20294 = DIRECTION ( 'NONE',  ( 0.000000000000000000, 0.000000000000000000, 1.000000000000000000 ) ) ;
#20295 = DIRECTION ( 'NONE',  ( -0.000000000000000000, -0.000000000000000000, 1.000000000000000000 ) ) ;
#20296 = ORIENTED_EDGE ( 'NONE', *, *, #6858, .T. ) ;
#20297 = ORIENTED_EDGE ( 'NONE', *, *, #13413, .T. ) ;
#20298 = CARTESIAN_POINT ( 'NONE',  ( 1.878215178125005158, 27.12812499938548783, 5.746835883940462963 ) ) ;
#20299 = ORIENTED_EDGE ( 'NONE', *, *, #8450, .F. ) ;
#20300 = CARTESIAN_POINT ( 'NONE',  ( 0.7500000000000001110, 9.184850993605150903E-17, 17.69999999999999929 ) ) ;
#20301 = ORIENTED_EDGE ( 'NONE', *, *, #22382, .T. ) ;
#20302 = CARTESIAN_POINT ( 'NONE',  ( 18.68225429291714690, -24.86329371854781201, -6.500000000000000000 ) ) ;
#20303 = ORIENTED_EDGE ( 'NONE', *, *, #17433, .F. ) ;
#20304 = CARTESIAN_POINT ( 'NONE',  ( 23.64116323484238080, 20.20656826142275264, 1.000000000000000000 ) ) ;
#20305 = ORIENTED_EDGE ( 'NONE', *, *, #21306, .F. ) ;
#20306 = DIRECTION ( 'NONE',  ( -0.000000000000000000, 1.000000000000000000, -0.000000000000000000 ) ) ;
#20307 = CARTESIAN_POINT ( 'NONE',  ( -1.878215178124995832, 26.64062499938548711, 5.746835883940462963 ) ) ;
#20308 = FACE_OUTER_BOUND ( 'NONE', #25083, .T. ) ;
#20309 = ADVANCED_FACE ( 'NONE', ( #6450 ), #10493, .T. ) ;
#20310 = CARTESIAN_POINT ( 'NONE',  ( 3.469446951953614189E-15, 40.00000000000000000, 8.999999999999992895 ) ) ;
#20311 = CARTESIAN_POINT ( 'NONE',  ( 1.859271017917182139E-15, 29.33124999877096428, 12.99999999999999289 ) ) ;
#20312 = CARTESIAN_POINT ( 'NONE',  ( -3.999999999999999556, 29.31250000000000000, 11.30940107675849404 ) ) ;
#20313 = EDGE_CURVE ( 'NONE', #4940, #10460, #7502, .T. ) ;
#20314 = CARTESIAN_POINT ( 'NONE',  ( 3.756430356250003655, 27.39062499938548356, 8.999999999999992895 ) ) ;
#20315 = EDGE_CURVE ( 'NONE', #17398, #13890, #25463, .T. ) ;
#20316 = CARTESIAN_POINT ( 'NONE',  ( -1.999999999999998224, 26.20000000000000284, 12.46410161513774639 ) ) ;
#20317 = CARTESIAN_POINT ( 'NONE',  ( 21.69050051289738690, 18.86207338815112067, 5.535898384862238508 ) ) ;
#20318 = ADVANCED_FACE ( 'NONE', ( #10623, #22276 ), #16263, .F. ) ;
#20319 = CARTESIAN_POINT ( 'NONE',  ( -3.999999999999996447, 29.27500000000000213, 8.999999999999992895 ) ) ;
#20320 = DIRECTION ( 'NONE',  ( 0.000000000000000000, 0.000000000000000000, 1.000000000000000000 ) ) ;
#20321 = AXIS2_PLACEMENT_3D ( 'NONE', #10002, #20320, #24510 ) ;
#20322 = CARTESIAN_POINT ( 'NONE',  ( -0.5000000000000000000, 6.000000000000000000, 19.50000000000000000 ) ) ;
#20323 = DIRECTION ( 'NONE',  ( 0.000000000000000000, -1.000000000000000000, 0.000000000000000000 ) ) ;
#20324 = ORIENTED_EDGE ( 'NONE', *, *, #20821, .F. ) ;
#20325 = CARTESIAN_POINT ( 'NONE',  ( 3.752267015613588906E-15, 28.20624999877096784, 4.381197846482986158 ) ) ;
#20326 = CARTESIAN_POINT ( 'NONE',  ( 1.500000000000001776, -7.499999999999993783, 25.00000000000000000 ) ) ;
#20328 = ORIENTED_EDGE ( 'NONE', *, *, #22579, .F. ) ;
#20327 = CARTESIAN_POINT ( 'NONE',  ( 3.756430356250000546, 28.36562499938548854, 11.16877607737301403 ) ) ;
#20329 = EDGE_LOOP ( 'NONE', ( #17888, #21108, #13657, #8096 ) ) ;
#20330 = CARTESIAN_POINT ( 'NONE',  ( -7.248980000273768098, 30.24338421796792176, -2.750000000000000000 ) ) ;
#20331 = CARTESIAN_POINT ( 'NONE',  ( 6.938893903907228378E-15, 29.50000000000000000, 3.499999999999992450 ) ) ;
#20332 = CARTESIAN_POINT ( 'NONE',  ( 1.626862140677534194E-14, 27.98124999877096997, 12.99999999999999289 ) ) ;
#20333 = ORIENTED_EDGE ( 'NONE', *, *, #9266, .F. ) ;
#20334 = EDGE_LOOP ( 'NONE', ( #5803, #17445, #21320, #14660 ) ) ;
#20335 = CARTESIAN_POINT ( 'NONE',  ( -3.756430356250003211, -26.64062499938548356, 6.831223922626973533 ) ) ;
#20336 = CARTESIAN_POINT ( 'NONE',  ( 1.878215178124998275, 28.21562499938549351, 12.25316411605952283 ) ) ;
#20337 = CARTESIAN_POINT ( 'NONE',  ( 1.057460391440397258E-14, -29.10624999877096641, 4.999999999999992006 ) ) ;
#20338 = CARTESIAN_POINT ( 'NONE',  ( 0.000000000000000000, 0.000000000000000000, 1.000000000000000000 ) ) ;
#20339 = EDGE_CURVE ( 'NONE', #25113, #10289, #2033, .T. ) ;
#20340 = CARTESIAN_POINT ( 'NONE',  ( 7.734255490827002255, 30.12293631110042469, 1.000000000000000000 ) ) ;
#20341 = PRODUCT_DEFINITION ( 'UNKNOWN', '', #13138, #3127 ) ;
#20342 = CARTESIAN_POINT ( 'NONE',  ( 6.317933499823437771, 30.45149776762727356, -2.750000000000000000 ) ) ;
#20343 = DIRECTION ( 'NONE',  ( 0.000000000000000000, 0.000000000000000000, 1.000000000000000000 ) ) ;
#20344 = CARTESIAN_POINT ( 'NONE',  ( 16.53304042674895058, 22.18989467624125922, 6.690598923241487306 ) ) ;
#20345 = FACE_OUTER_BOUND ( 'NONE', #13371, .T. ) ;
#20346 = CARTESIAN_POINT ( 'NONE',  ( 22.36900861179109867, 17.05661385587227841, 6.831223922626973533 ) ) ;
#20347 = CARTESIAN_POINT ( 'NONE',  ( 20.42212772327495784, 20.42212772327488324, 13.61880215351699874 ) ) ;
#20348 = EDGE_CURVE ( 'NONE', #8387, #24266, #9894, .T. ) ;
#20349 = PLANE ( 'NONE',  #21808 ) ;
#20350 = DIRECTION ( 'NONE',  ( 0.000000000000000000, 0.000000000000000000, 1.000000000000000000 ) ) ;
#20351 = CARTESIAN_POINT ( 'NONE',  ( 3.756430356250003655, 26.49062499938548498, 8.999999999999992895 ) ) ;
#20352 = EDGE_CURVE ( 'NONE', #12237, #24819, #5779, .T. ) ;
#20354 = ORIENTED_EDGE ( 'NONE', *, *, #12171, .F. ) ;
#20353 = CARTESIAN_POINT ( 'NONE',  ( -3.013274039476890653, 29.84885987243285399, 6.356496494711869616 ) ) ;
#20355 = CARTESIAN_POINT ( 'NONE',  ( 16.97933781724378122, 19.63553519520309010, 12.25316411605951927 ) ) ;
#20356 = CARTESIAN_POINT ( 'NONE',  ( 24.27856662945494293, -19.43607991388997291, -2.750000000000000000 ) ) ;
#20357 = VERTEX_POINT ( 'NONE', #6571 ) ;
#20358 = CYLINDRICAL_SURFACE ( 'NONE', #16772, 4.000000000000000000 ) ;
#20359 = CARTESIAN_POINT ( 'NONE',  ( 4.000000000000003553, 25.39374999877096784, 8.999999999999992895 ) ) ;
#20360 = CARTESIAN_POINT ( 'NONE',  ( -1.878215178125004048, -26.56562499938548427, 5.746835883940462963 ) ) ;
#20362 = VERTEX_POINT ( 'NONE', #8417 ) ;
#20361 = CARTESIAN_POINT ( 'NONE',  ( -1.999999999999995781, 25.15000000000000213, 5.535898384862237620 ) ) ;
#20363 = ORIENTED_EDGE ( 'NONE', *, *, #4360, .T. ) ;
#20364 = CARTESIAN_POINT ( 'NONE',  ( -3.756430356250002323, -26.90312499938548640, 11.16877607737301226 ) ) ;
#20365 = EDGE_LOOP ( 'NONE', ( #7375, #2363, #18224, #3140 ) ) ;
#20366 = VERTEX_POINT ( 'NONE', #20300 ) ;
#20367 = CARTESIAN_POINT ( 'NONE',  ( -31.03863125411927371, -1.952785157361310198, -6.500000000000000000 ) ) ;
#20368 = CARTESIAN_POINT ( 'NONE',  ( -3.753948939949354635, 38.72260848564138769, 13.39223537354781080 ) ) ;
#20369 = AXIS2_PLACEMENT_3D ( 'NONE', #15980, #17681, #21978 ) ;
#20370 = CARTESIAN_POINT ( 'NONE',  ( -16.16421332384701515, -26.25859848311253941, 1.000000000000000000 ) ) ;
#20371 = VECTOR ( 'NONE', #3736, 1000.000000000000227 ) ;
#20372 = CARTESIAN_POINT ( 'NONE',  ( -1.878215178124995832, -5.746835883940462963, 1.753124999385485827 ) ) ;
#20373 = CARTESIAN_POINT ( 'NONE',  ( -1.878215178124998497, 25.89062499938548356, 12.25316411605951927 ) ) ;
#20374 = CARTESIAN_POINT ( 'NONE',  ( 3.752267015613588906E-15, -4.381197846482986158, 1.856249998770964638 ) ) ;
#20375 = CARTESIAN_POINT ( 'NONE',  ( -1.999999999999995781, -5.535898384862237620, 3.750000000000000000 ) ) ;
#20376 = ADVANCED_FACE ( 'NONE', ( #16406 ), #12333, .F. ) ;
#20377 = CARTESIAN_POINT ( 'NONE',  ( -1.878215178124998497, 25.44062499938548427, 12.25316411605951927 ) ) ;
#20378 = CARTESIAN_POINT ( 'NONE',  ( 0.000000000000000000, 0.000000000000000000, 1.000000000000000000 ) ) ;
#20379 = FACE_OUTER_BOUND ( 'NONE', #5787, .T. ) ;
#20380 = CARTESIAN_POINT ( 'NONE',  ( 0.5000000000000000000, 0.8660254037844387076, 19.50000000000000000 ) ) ;
#20381 = CARTESIAN_POINT ( 'NONE',  ( 1.999999999999995781, -28.69374999877096855, 5.535898384862237620 ) ) ;
#20382 = CARTESIAN_POINT ( 'NONE',  ( 0.5000000000000001110, 10.00000000000000000, 13.00000000000000178 ) ) ;
#20383 = EDGE_CURVE ( 'NONE', #7744, #11788, #22532, .T. ) ;
#20384 = CARTESIAN_POINT ( 'NONE',  ( 1.626862140677534194E-14, 28.03750000000000497, 12.99999999999999289 ) ) ;
#20385 = AXIS2_PLACEMENT_3D ( 'NONE', #15293, #923, #10838 ) ;
#20386 = DIRECTION ( 'NONE',  ( 0.000000000000000000, 0.000000000000000000, 1.000000000000000000 ) ) ;
#20387 = CARTESIAN_POINT ( 'NONE',  ( 0.5247320085691752345, -29.99650235037416834, 5.025996973432255821 ) ) ;
#20388 = ORIENTED_EDGE ( 'NONE', *, *, #9765, .T. ) ;
#20389 = CARTESIAN_POINT ( 'NONE',  ( 4.000000000000003553, -8.999999999999992895, 18.00000000000000000 ) ) ;
#20391 = ORIENTED_EDGE ( 'NONE', *, *, #19884, .T. ) ;
#20390 = DIRECTION ( 'NONE',  ( 1.000000000000000000, 0.000000000000000000, 0.000000000000000000 ) ) ;
#20392 = ORIENTED_EDGE ( 'NONE', *, *, #21512, .T. ) ;
#20394 = ORIENTED_EDGE ( 'NONE', *, *, #12094, .T. ) ;
#20393 = VECTOR ( 'NONE', #5341, 1000.000000000000000 ) ;
#20395 = ORIENTED_EDGE ( 'NONE', *, *, #17247, .F. ) ;
#20396 = ORIENTED_EDGE ( 'NONE', *, *, #25360, .T. ) ;
#20397 = ORIENTED_EDGE ( 'NONE', *, *, #5478, .F. ) ;
#20398 = CARTESIAN_POINT ( 'NONE',  ( -21.28941499438242246, -22.67092431280570963, 1.000000000000000000 ) ) ;
#20399 = ORIENTED_EDGE ( 'NONE', *, *, #22417, .F. ) ;
#20400 = CYLINDRICAL_SURFACE ( 'NONE', #17780, 6.000000000000000888 ) ;
#20401 = CARTESIAN_POINT ( 'NONE',  ( 1.878215178125000939, 26.07812499938548356, 12.25316411605952283 ) ) ;
#20402 = AXIS2_PLACEMENT_3D ( 'NONE', #410, #2751, #20670 ) ;
#20403 = CARTESIAN_POINT ( 'NONE',  ( 2.672651547586948120E-15, -13.33755215474602984, 1.940624999385484717 ) ) ;
#20404 = AXIS2_PLACEMENT_3D ( 'NONE', #2705, #4670, #18657 ) ;
#20405 = CARTESIAN_POINT ( 'NONE',  ( 4.000000000000003553, -6.690598923241489970, 0.4312499987709677018 ) ) ;
#20406 = CARTESIAN_POINT ( 'NONE',  ( 22.05081056025715114, 16.73841580433833442, 6.831223922626973533 ) ) ;
#20407 = DIRECTION ( 'NONE',  ( 0.000000000000000000, 0.000000000000000000, 1.000000000000000000 ) ) ;
#20408 = CYLINDRICAL_SURFACE ( 'NONE', #24231, 4.000000000000000000 ) ;
#20409 = VECTOR ( 'NONE', #10039, 1000.000000000000000 ) ;
#20410 = CARTESIAN_POINT ( 'NONE',  ( -3.756430356249997882, -11.16877607737301226, 0.8531249993854844726 ) ) ;
#20411 = CARTESIAN_POINT ( 'NONE',  ( -1.999999999999998224, -12.46410161513774639, 4.349999999999999645 ) ) ;
#20412 = LINE ( 'NONE', #18482, #23461 ) ;
#20413 = ADVANCED_FACE ( 'NONE', ( #22142 ), #4761, .F. ) ;
#20414 = DIRECTION ( 'NONE',  ( 0.8660254037844397068, 0.4999999999999983347, -0.000000000000000000 ) ) ;
#20415 = CARTESIAN_POINT ( 'NONE',  ( -1.878215178124995832, -5.746835883940462963, 0.8531249993854843616 ) ) ;
#20416 = CARTESIAN_POINT ( 'NONE',  ( -8.831537335106614961E-15, -26.63124999877096855, 12.99999999999999112 ) ) ;
#20417 = CARTESIAN_POINT ( 'NONE',  ( -4.000000000000003553, -28.15000000000000213, 8.999999999999992895 ) ) ;
#20418 = EDGE_LOOP ( 'NONE', ( #25325, #6668, #6323 ) ) ;
#20419 = ORIENTED_EDGE ( 'NONE', *, *, #22936, .T. ) ;
#20420 = CARTESIAN_POINT ( 'NONE',  ( -1.878215178124996498, 28.55312499938548854, 5.746835883940462963 ) ) ;
#20421 = EDGE_CURVE ( 'NONE', #22705, #11048, #4614, .T. ) ;
#20422 = EDGE_CURVE ( 'NONE', #14523, #2078, #22496, .T. ) ;
#20423 = ORIENTED_EDGE ( 'NONE', *, *, #7955, .F. ) ;
#20424 = DIRECTION ( 'NONE',  ( 0.000000000000000000, 0.000000000000000000, 1.000000000000000000 ) ) ;
#20425 = ORIENTED_EDGE ( 'NONE', *, *, #7444, .T. ) ;
#20426 = CARTESIAN_POINT ( 'NONE',  ( 0.000000000000000000, 0.000000000000000000, 1.000000000000000000 ) ) ;
#20427 = ORIENTED_EDGE ( 'NONE', *, *, #6643, .T. ) ;
#20428 = DIRECTION ( 'NONE',  ( 0.000000000000000000, 0.000000000000000000, -1.000000000000000000 ) ) ;
#20429 = AXIS2_PLACEMENT_3D ( 'NONE', #10215, #24083, #11804 ) ;
#20430 = EDGE_CURVE ( 'NONE', #9082, #8835, #11207, .T. ) ;
#20431 = CYLINDRICAL_SURFACE ( 'NONE', #16955, 0.5000000000000004441 ) ;
#20432 = AXIS2_PLACEMENT_3D ( 'NONE', #20452, #20597, #8305 ) ;
#20433 = ORIENTED_EDGE ( 'NONE', *, *, #14305, .T. ) ;
#20434 = CARTESIAN_POINT ( 'NONE',  ( 27.00874656207304980, 15.41874213889405176, -6.500000000000000000 ) ) ;
#20435 =( BOUNDED_CURVE ( )  B_SPLINE_CURVE ( 2, ( #22583, #22718, #4519, #353, #12774, #6367, #737 ),
 .UNSPECIFIED., .F., .F. ) 
 B_SPLINE_CURVE_WITH_KNOTS ( ( 3, 2, 2, 3 ),
 ( 0.2000000000000003719, 0.2166666666666670071, 0.2333333333333336423, 0.2500000000000002776 ),
 .UNSPECIFIED. ) 
 CURVE ( )  GEOMETRIC_REPRESENTATION_ITEM ( )  RATIONAL_B_SPLINE_CURVE ( ( 0.9999999999999971134, 0.8660254037844415942, 1.000000000000000000, 0.8660254037844387076, 1.000000000000000000, 0.8660254037844364872, 1.000000000000002220 ) ) 
 REPRESENTATION_ITEM ( '' )  );
#20436 = CARTESIAN_POINT ( 'NONE',  ( 3.756430356250003655, 26.94062499938548427, 8.999999999999992895 ) ) ;
#20437 = CARTESIAN_POINT ( 'NONE',  ( -25.75859848311282363, -16.66421332384654974, 1.000000000000000000 ) ) ;
#20438 = VECTOR ( 'NONE', #667, 1000.000000000000000 ) ;
#20439 = CARTESIAN_POINT ( 'NONE',  ( 0.000000000000000000, 0.000000000000000000, 1.000000000000000000 ) ) ;
#20440 = CARTESIAN_POINT ( 'NONE',  ( 0.000000000000000000, 0.000000000000000000, -6.500000000000000000 ) ) ;
#20441 = CARTESIAN_POINT ( 'NONE',  ( 4.000000000000002665, 29.46250000000000568, 11.30940107675849760 ) ) ;
#20442 =( BOUNDED_CURVE ( )  B_SPLINE_CURVE ( 2, ( #16749, #2625, #16496, #14654, #2747, #4323, #10709, #18696, #20265 ),
 .UNSPECIFIED., .F., .F. ) 
 B_SPLINE_CURVE_WITH_KNOTS ( ( 3, 2, 2, 2, 3 ),
 ( 0.6250000000000000000, 0.6333333333333333037, 0.6500000000000000222, 0.6666666666666666297, 0.6750000000000000444 ),
 .UNSPECIFIED. ) 
 CURVE ( )  GEOMETRIC_REPRESENTATION_ITEM ( )  RATIONAL_B_SPLINE_CURVE ( ( 0.9330127018922194093, 0.9330127018922194093, 1.000000000000000000, 0.8660254037844387076, 1.000000000000000000, 0.8660254037844387076, 1.000000000000000000, 0.9330127018922189652, 0.9330127018922194093 ) ) 
 REPRESENTATION_ITEM ( '' )  );
#20443 = CIRCLE ( 'NONE', #19191, 0.5000000000000011102 ) ;
#20444 = AXIS2_PLACEMENT_3D ( 'NONE', #757, #14883, #9111 ) ;
#20445 = CARTESIAN_POINT ( 'NONE',  ( -3.756430356249995661, 27.57812499938548356, 6.831223922626973533 ) ) ;
#20446 = PRESENTATION_LAYER_ASSIGNMENT (  '', '', ( #17533 ) ) ;
#20447 = DIRECTION ( 'NONE',  ( 0.000000000000000000, 0.000000000000000000, 1.000000000000000000 ) ) ;
#20448 = CARTESIAN_POINT ( 'NONE',  ( 17.89864039878453283, 23.55549464827683437, 11.30940107675849404 ) ) ;
#20449 = DIRECTION ( 'NONE',  ( 0.000000000000000000, -1.000000000000000000, 0.000000000000000000 ) ) ;
#20450 = CARTESIAN_POINT ( 'NONE',  ( 1.878215178124998497, -28.59062499938548285, 12.25316411605951927 ) ) ;
#20451 = EDGE_CURVE ( 'NONE', #4678, #4202, #23800, .T. ) ;
#20452 = CARTESIAN_POINT ( 'NONE',  ( -3.897863563850083146, -30.85476721088024021, -6.500000000000000000 ) ) ;
#20453 = AXIS2_PLACEMENT_3D ( 'NONE', #21380, #5796, #3704 ) ;
#20454 = VERTEX_POINT ( 'NONE', #25007 ) ;
#20455 = CARTESIAN_POINT ( 'NONE',  ( 3.756430356250003655, 25.70312499938548356, 8.999999999999992895 ) ) ;
#20456 = CARTESIAN_POINT ( 'NONE',  ( -2.000000000000003997, -29.12500000000000000, 5.535898384862238508 ) ) ;
#20458 = ORIENTED_EDGE ( 'NONE', *, *, #17316, .T. ) ;
#20457 = CARTESIAN_POINT ( 'NONE',  ( 3.756430356250004099, 26.64062499938549422, 6.831223922626973533 ) ) ;
#20459 = ORIENTED_EDGE ( 'NONE', *, *, #7590, .T. ) ;
#20460 = CARTESIAN_POINT ( 'NONE',  ( 1.859271017917182139E-15, 28.88124999877096499, 12.99999999999999289 ) ) ;
#20461 = AXIS2_PLACEMENT_3D ( 'NONE', #7461, #23286, #19755 ) ;
#20462 = EDGE_CURVE ( 'NONE', #12917, #23846, #21211, .T. ) ;
#20463 = DIRECTION ( 'NONE',  ( 0.000000000000000000, 0.000000000000000000, 1.000000000000000000 ) ) ;
#20464 = CARTESIAN_POINT ( 'NONE',  ( -1.999999999999995781, 25.54374999877096997, 5.535898384862237620 ) ) ;
#20465 = EDGE_CURVE ( 'NONE', #2390, #17829, #4875, .T. ) ;
#20466 = ORIENTED_EDGE ( 'NONE', *, *, #5687, .F. ) ;
#20467 = ORIENTED_EDGE ( 'NONE', *, *, #10589, .T. ) ;
#20468 = CARTESIAN_POINT ( 'NONE',  ( -1.878215178125000939, -27.87812499938548427, 12.25316411605952283 ) ) ;
#20469 = CARTESIAN_POINT ( 'NONE',  ( -3.756430356249996105, 27.57812499938548356, 6.831223922626973533 ) ) ;
#20470 = CARTESIAN_POINT ( 'NONE',  ( 19.30843454290614147, 19.30843454290607752, 4.999999999999991118 ) ) ;
#20471 = VECTOR ( 'NONE', #25129, 1000.000000000000000 ) ;
#20472 = DIRECTION ( 'NONE',  ( -1.000000000000000000, 2.891205793294678326E-16, 0.000000000000000000 ) ) ;
#20473 = ADVANCED_FACE ( 'NONE', ( #1347 ), #3290, .F. ) ;
#20474 = AXIS2_PLACEMENT_3D ( 'NONE', #14947, #17039, #7233 ) ;
#20475 = CYLINDRICAL_SURFACE ( 'NONE', #25462, 4.000000000000000000 ) ;
#20476 = CARTESIAN_POINT ( 'NONE',  ( 0.000000000000000000, 0.000000000000000000, 0.000000000000000000 ) ) ;
#20477 = CARTESIAN_POINT ( 'NONE',  ( 3.999999999999997335, -28.41250000000000142, 11.30940107675849404 ) ) ;
#20478 = AXIS2_PLACEMENT_3D ( 'NONE', #24568, #20658, #19074 ) ;
#20479 = AXIS2_PLACEMENT_3D ( 'NONE', #21877, #7490, #15481 ) ;
#20480 = CARTESIAN_POINT ( 'NONE',  ( -1.499999999999998224, -10.49999999999999289, 25.00000000000000000 ) ) ;
#20481 = DIRECTION ( 'NONE',  ( 1.000000000000000000, 0.000000000000000000, 0.000000000000000000 ) ) ;
#20482 = LINE ( 'NONE', #12778, #11205 ) ;
#20484 = EDGE_CURVE ( 'NONE', #19902, #16230, #4946, .T. ) ;
#20483 = CARTESIAN_POINT ( 'NONE',  ( 21.41441445718925962, 16.10201970127043936, 6.831223922626973533 ) ) ;
#20485 = CARTESIAN_POINT ( 'NONE',  ( 21.86285778994254514, 19.03443066519628601, 12.46410161513774817 ) ) ;
#20486 = VECTOR ( 'NONE', #19666, 1000.000000000000000 ) ;
#20487 = LINE ( 'NONE', #24536, #1771 ) ;
#20488 = CARTESIAN_POINT ( 'NONE',  ( -13.24173596767398742, -28.14012133169310559, -6.500000000000000000 ) ) ;
#20489 = CARTESIAN_POINT ( 'NONE',  ( 2.672651547586948120E-15, 26.37812499938548427, 13.33755215474602984 ) ) ;
#20490 = AXIS2_PLACEMENT_3D ( 'NONE', #16091, #25760, #19752 ) ;
#20492 = VERTEX_POINT ( 'NONE', #2782 ) ;
#20491 = CARTESIAN_POINT ( 'NONE',  ( -3.470226642398214878, 29.79897209676519765, 11.00633161724385900 ) ) ;
#20493 = CARTESIAN_POINT ( 'NONE',  ( 15.28000806814115720, 20.59240282405983535, 8.999999999999992895 ) ) ;
#20494 = CARTESIAN_POINT ( 'NONE',  ( -3.999999999999959144, -11.30940107675851891, 1.162499999999999423 ) ) ;
#20495 = ORIENTED_EDGE ( 'NONE', *, *, #20465, .T. ) ;
#20496 = FACE_OUTER_BOUND ( 'NONE', #3313, .T. ) ;
#20497 = DIRECTION ( 'NONE',  ( -0.2486898871648449971, 0.9685831611286336296, 0.000000000000000000 ) ) ;
#20498 = CARTESIAN_POINT ( 'NONE',  ( 3.756430356249996994, -25.81562499938548427, 8.999999999999992895 ) ) ;
#20500 = VERTEX_POINT ( 'NONE', #19249 ) ;
#20499 = CARTESIAN_POINT ( 'NONE',  ( 21.28941499438225904, 22.67092431280586240, 1.000000000000000000 ) ) ;
#20501 = CARTESIAN_POINT ( 'NONE',  ( 17.92837382773583954, 19.44412335558781280, 4.999999999999992006 ) ) ;
#20502 = ADVANCED_FACE ( 'NONE', ( #14945 ), #963, .F. ) ;
#20503 = AXIS2_PLACEMENT_3D ( 'NONE', #8170, #19532, #20712 ) ;
#20504 = VERTEX_POINT ( 'NONE', #11136 ) ;
#20505 = CARTESIAN_POINT ( 'NONE',  ( -1.878215178125004048, -26.56562499938548427, 5.746835883940462963 ) ) ;
#20506 = ORIENTED_EDGE ( 'NONE', *, *, #11274, .F. ) ;
#20507 = ORIENTED_EDGE ( 'NONE', *, *, #20030, .T. ) ;
#20508 = EDGE_CURVE ( 'NONE', #7703, #25247, #4524, .T. ) ;
#20509 = DIRECTION ( 'NONE',  ( 0.000000000000000000, 0.000000000000000000, 1.000000000000000000 ) ) ;
#20510 = VECTOR ( 'NONE', #17091, 1000.000000000000000 ) ;
#20511 = CARTESIAN_POINT ( 'NONE',  ( -3.756430356249998326, 25.51562499938549067, 11.16877607737301226 ) ) ;
#20512 = VECTOR ( 'NONE', #11353, 1000.000000000000000 ) ;
#20513 = CARTESIAN_POINT ( 'NONE',  ( -17.78012134629613783, -25.16042852506070560, -6.500000000000000000 ) ) ;
#20514 = EDGE_CURVE ( 'NONE', #20798, #19181, #24760, .T. ) ;
#20515 = AXIS2_PLACEMENT_3D ( 'NONE', #742, #10793, #4525 ) ;
#20516 = CARTESIAN_POINT ( 'NONE',  ( -1.878215178124998497, -12.25316411605951927, 1.453124999385484228 ) ) ;
#20517 =( NAMED_UNIT ( * ) SI_UNIT ( $, .STERADIAN. ) SOLID_ANGLE_UNIT ( ) );
#20518 = CARTESIAN_POINT ( 'NONE',  ( 30.24338421796784004, 7.248980000274092284, -6.500000000000000000 ) ) ;
#20519 = CARTESIAN_POINT ( 'NONE',  ( 2.672651547586948120E-15, 25.92812499938548498, 13.33755215474602984 ) ) ;
#20520 = CARTESIAN_POINT ( 'NONE',  ( 23.36987911821542951, 17.71302486872297166, 8.999999999999992895 ) ) ;
#20521 = CIRCLE ( 'NONE', #22189, 26.00000000000000711 ) ;
#20522 = CARTESIAN_POINT ( 'NONE',  ( 0.000000000000000000, 0.000000000000000000, -6.500000000000000000 ) ) ;
#20523 = CARTESIAN_POINT ( 'NONE',  ( -3.756430356249996105, 26.67812499938548498, 6.831223922626973533 ) ) ;
#20524 = FILL_AREA_STYLE_COLOUR ( '', #2110 ) ;
#20525 = DIRECTION ( 'NONE',  ( 0.000000000000000000, 1.000000000000000000, 0.000000000000000000 ) ) ;
#20526 = CARTESIAN_POINT ( 'NONE',  ( -30.24338421796775123, 7.248980000274508839, 1.000000000000000000 ) ) ;
#20527 = CARTESIAN_POINT ( 'NONE',  ( 3.756430356249997882, -25.96562499938548640, 11.16877607737301226 ) ) ;
#20528 = SHAPE_REPRESENTATION ( 'dust cap', ( #21036 ), #8945 ) ;
#20529 = VECTOR ( 'NONE', #14456, 1000.000000000000000 ) ;
#20530 = CARTESIAN_POINT ( 'NONE',  ( 20.20656826142283435, 23.64116323484230975, -2.750000000000000000 ) ) ;
#20531 = CARTESIAN_POINT ( 'NONE',  ( -4.000000000000026645, -6.690598923241505958, 2.887499999999999734 ) ) ;
#20532 = CARTESIAN_POINT ( 'NONE',  ( 1.500000000000001776, -10.49999999999999289, -6.938893903907228378E-15 ) ) ;
#20533 = CARTESIAN_POINT ( 'NONE',  ( 3.871674220476135631, -29.74916513505594295, 7.961019890438434388 ) ) ;
#20534 = ORIENTED_EDGE ( 'NONE', *, *, #925, .T. ) ;
#20535 = FACE_OUTER_BOUND ( 'NONE', #9450, .T. ) ;
#20537 = ORIENTED_EDGE ( 'NONE', *, *, #17726, .T. ) ;
#20536 = CARTESIAN_POINT ( 'NONE',  ( -3.469446951953614189E-15, -30.00000000000000355, 8.999999999999992895 ) ) ;
#20538 = CIRCLE ( 'NONE', #21384, 6.000000000000000000 ) ;
#20539 = VERTEX_POINT ( 'NONE', #25144 ) ;
#20540 = EDGE_LOOP ( 'NONE', ( #6638, #16859, #17449 ) ) ;
#20541 = ORIENTED_EDGE ( 'NONE', *, *, #10839, .F. ) ;
#20542 = ORIENTED_EDGE ( 'NONE', *, *, #1541, .T. ) ;
#20543 = ORIENTED_EDGE ( 'NONE', *, *, #24716, .F. ) ;
#20544 = LINE ( 'NONE', #10465, #20985 ) ;
#20545 = CIRCLE ( 'NONE', #23455, 0.5000000000000011102 ) ;
#20546 = VERTEX_POINT ( 'NONE', #24886 ) ;
#20547 = EDGE_CURVE ( 'NONE', #20076, #24433, #7102, .T. ) ;
#20548 = CARTESIAN_POINT ( 'NONE',  ( 16.66421332384664566, -26.25859848311276679, -6.500000000000000000 ) ) ;
#20549 = CARTESIAN_POINT ( 'NONE',  ( -3.756430356249997438, 28.21562499938548640, 11.16877607737301048 ) ) ;
#20550 = CIRCLE ( 'NONE', #23894, 31.10000000000000142 ) ;
#20551 = ADVANCED_FACE ( 'NONE', ( #6964 ), #16790, .F. ) ;
#20552 = CARTESIAN_POINT ( 'NONE',  ( -3.756430356249997882, -11.16877607737301226, 2.315624999385482496 ) ) ;
#20553 = CARTESIAN_POINT ( 'NONE',  ( 3.959305671612554781E-15, 40.00000000000000000, 12.99999999999999289 ) ) ;
#20554 = CARTESIAN_POINT ( 'NONE',  ( 18.88852612644745932, 21.54472350440676109, 12.25316411605951927 ) ) ;
#20555 = ADVANCED_FACE ( 'NONE', ( #15213 ), #5005, .F. ) ;
#20556 = AXIS2_PLACEMENT_3D ( 'NONE', #4516, #10535, #7270 ) ;
#20557 = DIRECTION ( 'NONE',  ( -0.000000000000000000, -0.000000000000000000, 1.000000000000000000 ) ) ;
#20558 = ADVANCED_FACE ( 'NONE', ( #23300, #12730 ), #13241, .T. ) ;
#20559 = CARTESIAN_POINT ( 'NONE',  ( 4.000000000000030198, -6.690598923241506846, 0.4874999999999962697 ) ) ;
#20560 = CARTESIAN_POINT ( 'NONE',  ( 3.756430356250004099, -6.831223922626973533, 2.878124999385481608 ) ) ;
#20561 = DIRECTION ( 'NONE',  ( 0.000000000000000000, 0.000000000000000000, 1.000000000000000000 ) ) ;
#20562 = CARTESIAN_POINT ( 'NONE',  ( 3.469446951953614189E-15, 30.00000000000000355, 8.999999999999992895 ) ) ;
#20563 = CARTESIAN_POINT ( 'NONE',  ( 6.972266317189432034E-15, 28.65624999877097423, 4.999999999999992006 ) ) ;
#20564 = CYLINDRICAL_SURFACE ( 'NONE', #9645, 0.5000000000000004441 ) ;
#20565 = CARTESIAN_POINT ( 'NONE',  ( 3.756430356250003655, -8.999999999999992895, 2.503124999385482941 ) ) ;
#20566 = DIRECTION ( 'NONE',  ( 0.000000000000000000, 0.000000000000000000, 1.000000000000000000 ) ) ;
#20567 = AXIS2_PLACEMENT_3D ( 'NONE', #9157, #19218, #17016 ) ;
#20568 = ORIENTED_EDGE ( 'NONE', *, *, #4253, .F. ) ;
#20569 = ORIENTED_EDGE ( 'NONE', *, *, #9173, .T. ) ;
#20570 = CARTESIAN_POINT ( 'NONE',  ( 1.878215178124999829, 28.32812499938549422, 12.25316411605952283 ) ) ;
#20571 = VECTOR ( 'NONE', #16643, 1000.000000000000000 ) ;
#20572 = ORIENTED_EDGE ( 'NONE', *, *, #3464, .F. ) ;
#20573 = DIRECTION ( 'NONE',  ( -0.1873813145857119722, 0.9822872507286911636, 0.000000000000000000 ) ) ;
#20574 = ORIENTED_EDGE ( 'NONE', *, *, #15919, .T. ) ;
#20575 = CARTESIAN_POINT ( 'NONE',  ( -3.999999999999996447, 28.33750000000000568, 6.690598923241487306 ) ) ;
#20576 = VERTEX_POINT ( 'NONE', #3049 ) ;
#20577 = CARTESIAN_POINT ( 'NONE',  ( -3.999999999999996447, 27.83124999877097139, 6.690598923241487306 ) ) ;
#20578 = CARTESIAN_POINT ( 'NONE',  ( 0.000000000000000000, 0.000000000000000000, 1.000000000000000000 ) ) ;
#20579 = ORIENTED_EDGE ( 'NONE', *, *, #1144, .F. ) ;
#20580 = CARTESIAN_POINT ( 'NONE',  ( -0.4995657836784084815, 34.50000000000000000, 14.97916666666665897 ) ) ;
#20581 = CARTESIAN_POINT ( 'NONE',  ( 4.000000000000003553, 25.48750000000000071, 6.690598923241489970 ) ) ;
#20582 = CARTESIAN_POINT ( 'NONE',  ( 16.30765014111479161, 21.96450439060710025, 11.30940107675849404 ) ) ;
#20583 = ADVANCED_FACE ( 'NONE', ( #17037 ), #13120, .T. ) ;
#20584=STYLED_ITEM('',(#25907),#4802);
#20585 = CYLINDRICAL_SURFACE ( 'NONE', #21355, 4.000000000000000000 ) ;
#20586 = CARTESIAN_POINT ( 'NONE',  ( 17.96814858504663448, 19.48389811289862195, 4.999999999999992895 ) ) ;
#20587 = CARTESIAN_POINT ( 'NONE',  ( 15.38607408531914089, 20.69846884123782260, 11.16877607737301226 ) ) ;
#20588 = AXIS2_PLACEMENT_3D ( 'NONE', #17005, #1050, #17274 ) ;
#20589 = CARTESIAN_POINT ( 'NONE',  ( -1.878215178124995832, 28.89062499938548356, 5.746835883940462963 ) ) ;
#20590 = EDGE_CURVE ( 'NONE', #8694, #16529, #22964, .T. ) ;
#20591 = DIRECTION ( 'NONE',  ( 0.000000000000000000, 0.000000000000000000, 1.000000000000000000 ) ) ;
#20592 = CIRCLE ( 'NONE', #20157, 31.10000000000000142 ) ;
#20593 = CARTESIAN_POINT ( 'NONE',  ( 23.34336261392093448, 17.68650836442847663, 11.30940107675849760 ) ) ;
#20594 = CARTESIAN_POINT ( 'NONE',  ( 0.000000000000000000, 26.18124999877096926, 13.61880215351699874 ) ) ;
#20595 = CARTESIAN_POINT ( 'NONE',  ( 25.98730014090430274, -17.08421000182786997, -2.750000000000000000 ) ) ;
#20596 = CARTESIAN_POINT ( 'NONE',  ( -3.756430356250002323, -26.45312499938548356, 11.16877607737301403 ) ) ;
#20597 = DIRECTION ( 'NONE',  ( 0.000000000000000000, 0.000000000000000000, 1.000000000000000000 ) ) ;
#20598 = VERTEX_POINT ( 'NONE', #1203 ) ;
#20599 = CARTESIAN_POINT ( 'NONE',  ( 4.000000000000003553, 29.03124999877096712, 6.690598923241489970 ) ) ;
#20600 = CARTESIAN_POINT ( 'NONE',  ( 21.01432965251868978, 18.18590252777242711, 5.535898384862238508 ) ) ;
#20602 = VERTEX_POINT ( 'NONE', #9186 ) ;
#20601 = CARTESIAN_POINT ( 'NONE',  ( -3.756430356250000546, 29.56562499938549493, 11.16877607737301048 ) ) ;
#20603 = VERTEX_POINT ( 'NONE', #17176 ) ;
#20604 =( BOUNDED_SURFACE ( )  B_SPLINE_SURFACE ( 1, 2, ( 
 ( #16770, #20405, #12966, #14806, #20947, #18855, #8533, #16514, #24476, #17289, #25504, #3269, #23546, #15441, #13222, #11244, #1711, #21192, #19359, #19224, #5499, #1573, #3153, #21328, #15578, #17152, #3537, #25638, #1324, #11119, #23414, #9304, #3406, #7211, #5126, #19608, #13492, #11631, #1182, #25254, #13352, #19098, #9162, #21076, #7333, #15313, #9684, #7454, #21460, #9544, #25123, #17530, #15063, #15193, #17405, #11384, #23163, #23038, #5243, #23281, #1454, #17670, #25370, #13102, #11508, #5363, #9425, #19479, #7593, #5629, #13610, #21575, #3654, #21967, #9808, #10185, #25756, #6136, #12152, #20126, #17790, #21842, #1961, #23668, #22085, #18183, #7838, #13994, #2228, #3923, #15822, #23932, #12010, #5883, #23794, #11894, #11769, #13867, #7978, #6014, #19863, #24052, #6267, #19987, #2092, #14259, #19747, #5745, #18058, #9925, #3, #7719, #266, #15702, #17912, #3792, #18299, #4043, #22226, #10058, #15964 ),
 ( #16089, #4311, #142, #8115, #14121, #13726, #16211, #4174, #8232, #24179, #12286, #20251, #2349, #10304, #21707, #1846, #8887, #770, #24444, #22477, #12929, #6521, #4706, #14505, #16732, #4948, #652, #10571, #20776, #10964, #8500, #22347, #20516, #18818, #4556, #22868, #14894, #4432, #12539, #12405, #20372, #908, #6788, #18570, #6649, #8620, #2612, #16599, #12802, #10695, #24703, #392, #16870, #24560, #16482, #14391, #14637, #22617, #20908, #12679, #2995, #2467, #8361, #2855, #20650, #2732, #18682, #8742, #10824, #14773, #24836, #10440, #6911, #22748, #4825, #16350, #24319, #6399, #18434, #528, #21542, #5214, #5463, #7177, #15023, #9510, #7554, #11209, #23379, #25225, #19451, #3506, #17492, #21425, #25467, #13068, #7305, #19067, #15544, #1542, #1034, #17376, #5332, #3371, #13457, #25091, #5598, #15165, #7036, #25341, #17116, #23512, #18949, #3625, #15281, #7420, #21046, #11476, #23002, #13577, #23247 ) ),
 .UNSPECIFIED., .F., .F., .T. ) 
 B_SPLINE_SURFACE_WITH_KNOTS ( ( 2, 2 ),
 ( 3, 2, 2, 2, 2, 2, 2, 2, 2, 2, 2, 2, 2, 2, 2, 2, 2, 2, 2, 2, 2, 2, 2, 2, 2, 2, 2, 2, 2, 2, 2, 2, 2, 2, 2, 2, 2, 2, 2, 2, 2, 2, 2, 2, 2, 2, 2, 2, 2, 2, 2, 2, 2, 2, 2, 2, 2, 2, 2, 2, 3 ),
 ( 0.000000000000000000, 1.000000000000000000 ),
 ( 0.000000000000000000, 0.01666666666666666644, 0.03333333333333333287, 0.05000000000000000278, 0.06666666666666666574, 0.08333333333333332871, 0.1000000000000000056, 0.1166666666666666685, 0.1333333333333333315, 0.1499999999999999944, 0.1666666666666666574, 0.1833333333333333204, 0.2000000000000000111, 0.2166666666666666741, 0.2333333333333333370, 0.2500000000000000000, 0.2666666666666666630, 0.2833333333333333259, 0.2999999999999999889, 0.3166666666666666519, 0.3333333333333333148, 0.3499999999999999778, 0.3666666666666666408, 0.3833333333333333592, 0.4000000000000000222, 0.4166666666666666852, 0.4333333333333333481, 0.4500000000000000111, 0.4666666666666666741, 0.4833333333333333370, 0.5000000000000000000, 0.5166666666666667185, 0.5333333333333333259, 0.5500000000000000444, 0.5666666666666666519, 0.5833333333333333703, 0.5999999999999999778, 0.6166666666666666963, 0.6333333333333333037, 0.6500000000000000222, 0.6666666666666666297, 0.6833333333333333481, 0.6999999999999999556, 0.7166666666666666741, 0.7333333333333332815, 0.7500000000000000000, 0.7666666666666667185, 0.7833333333333333259, 0.8000000000000000444, 0.8166666666666666519, 0.8333333333333333703, 0.8499999999999999778, 0.8666666666666666963, 0.8833333333333333037, 0.9000000000000000222, 0.9166666666666666297, 0.9333333333333333481, 0.9499999999999999556, 0.9666666666666666741, 0.9833333333333332815, 1.000000000000000000 ),
 .UNSPECIFIED. ) 
 GEOMETRIC_REPRESENTATION_ITEM ( )  RATIONAL_B_SPLINE_SURFACE ( (
 ( 1.000000000000000000, 0.8660254037844387076, 1.000000000000000000, 0.8660254037844387076, 1.000000000000000000, 0.8660254037844387076, 1.000000000000000000, 0.8660254037844387076, 1.000000000000000000, 0.8660254037844387076, 1.000000000000000000, 0.8660254037844387076, 1.000000000000000000, 0.8660254037844387076, 1.000000000000000000, 0.8660254037844387076, 1.000000000000000000, 0.8660254037844387076, 1.000000000000000000, 0.8660254037844387076, 1.000000000000000000, 0.8660254037844387076, 1.000000000000000000, 0.8660254037844387076, 1.000000000000000000, 0.8660254037844387076, 1.000000000000000000, 0.8660254037844387076, 1.000000000000000000, 0.8660254037844387076, 1.000000000000000000, 0.8660254037844387076, 1.000000000000000000, 0.8660254037844387076, 1.000000000000000000, 0.8660254037844387076, 1.000000000000000000, 0.8660254037844387076, 1.000000000000000000, 0.8660254037844387076, 1.000000000000000000, 0.8660254037844387076, 1.000000000000000000, 0.8660254037844387076, 1.000000000000000000, 0.8660254037844387076, 1.000000000000000000, 0.8660254037844387076, 1.000000000000000000, 0.8660254037844387076, 1.000000000000000000, 0.8660254037844387076, 1.000000000000000000, 0.8660254037844387076, 1.000000000000000000, 0.8660254037844387076, 1.000000000000000000, 0.8660254037844387076, 1.000000000000000000, 0.8660254037844387076, 1.000000000000000000, 0.8660254037844387076, 1.000000000000000000, 0.8660254037844387076, 1.000000000000000000, 0.8660254037844387076, 1.000000000000000000, 0.8660254037844387076, 1.000000000000000000, 0.8660254037844387076, 1.000000000000000000, 0.8660254037844387076, 1.000000000000000000, 0.8660254037844387076, 1.000000000000000000, 0.8660254037844387076, 1.000000000000000000, 0.8660254037844387076, 1.000000000000000000, 0.8660254037844387076, 1.000000000000000000, 0.8660254037844387076, 1.000000000000000000, 0.8660254037844387076, 1.000000000000000000, 0.8660254037844387076, 1.000000000000000000, 0.8660254037844387076, 1.000000000000000000, 0.8660254037844387076, 1.000000000000000000, 0.8660254037844387076, 1.000000000000000000, 0.8660254037844387076, 1.000000000000000000, 0.8660254037844387076, 1.000000000000000000, 0.8660254037844387076, 1.000000000000000000, 0.8660254037844387076, 1.000000000000000000, 0.8660254037844387076, 1.000000000000000000, 0.8660254037844387076, 1.000000000000000000, 0.8660254037844387076, 1.000000000000000000, 0.8660254037844387076, 1.000000000000000000, 0.8660254037844387076, 1.000000000000000000, 0.8660254037844387076, 1.000000000000000000, 0.8660254037844387076, 1.000000000000000000, 0.8660254037844387076, 1.000000000000000000, 0.8660254037844387076, 1.000000000000000000, 0.8660254037844387076, 1.000000000000000000),
 ( 1.000000000000000000, 0.8660254037844387076, 1.000000000000000000, 0.8660254037844387076, 1.000000000000000000, 0.8660254037844387076, 1.000000000000000000, 0.8660254037844387076, 1.000000000000000000, 0.8660254037844387076, 1.000000000000000000, 0.8660254037844387076, 1.000000000000000000, 0.8660254037844387076, 1.000000000000000000, 0.8660254037844387076, 1.000000000000000000, 0.8660254037844387076, 1.000000000000000000, 0.8660254037844387076, 1.000000000000000000, 0.8660254037844387076, 1.000000000000000000, 0.8660254037844387076, 1.000000000000000000, 0.8660254037844387076, 1.000000000000000000, 0.8660254037844387076, 1.000000000000000000, 0.8660254037844387076, 1.000000000000000000, 0.8660254037844387076, 1.000000000000000000, 0.8660254037844387076, 1.000000000000000000, 0.8660254037844387076, 1.000000000000000000, 0.8660254037844387076, 1.000000000000000000, 0.8660254037844387076, 1.000000000000000000, 0.8660254037844387076, 1.000000000000000000, 0.8660254037844387076, 1.000000000000000000, 0.8660254037844387076, 1.000000000000000000, 0.8660254037844387076, 1.000000000000000000, 0.8660254037844387076, 1.000000000000000000, 0.8660254037844387076, 1.000000000000000000, 0.8660254037844387076, 1.000000000000000000, 0.8660254037844387076, 1.000000000000000000, 0.8660254037844387076, 1.000000000000000000, 0.8660254037844387076, 1.000000000000000000, 0.8660254037844387076, 1.000000000000000000, 0.8660254037844387076, 1.000000000000000000, 0.8660254037844387076, 1.000000000000000000, 0.8660254037844387076, 1.000000000000000000, 0.8660254037844387076, 1.000000000000000000, 0.8660254037844387076, 1.000000000000000000, 0.8660254037844387076, 1.000000000000000000, 0.8660254037844387076, 1.000000000000000000, 0.8660254037844387076, 1.000000000000000000, 0.8660254037844387076, 1.000000000000000000, 0.8660254037844387076, 1.000000000000000000, 0.8660254037844387076, 1.000000000000000000, 0.8660254037844387076, 1.000000000000000000, 0.8660254037844387076, 1.000000000000000000, 0.8660254037844387076, 1.000000000000000000, 0.8660254037844387076, 1.000000000000000000, 0.8660254037844387076, 1.000000000000000000, 0.8660254037844387076, 1.000000000000000000, 0.8660254037844387076, 1.000000000000000000, 0.8660254037844387076, 1.000000000000000000, 0.8660254037844387076, 1.000000000000000000, 0.8660254037844387076, 1.000000000000000000, 0.8660254037844387076, 1.000000000000000000, 0.8660254037844387076, 1.000000000000000000, 0.8660254037844387076, 1.000000000000000000, 0.8660254037844387076, 1.000000000000000000, 0.8660254037844387076, 1.000000000000000000, 0.8660254037844387076, 1.000000000000000000, 0.8660254037844387076, 1.000000000000000000, 0.8660254037844387076, 1.000000000000000000) ) ) 
 REPRESENTATION_ITEM ( '' )  SURFACE ( )  );
#20605 = CARTESIAN_POINT ( 'NONE',  ( -1.999999999999996669, -8.999999999999992895, 6.000000000000000000 ) ) ;
#20606 = CARTESIAN_POINT ( 'NONE',  ( 3.959305671612554781E-15, 35.50000000000000711, 12.99999999999999289 ) ) ;
#20607 = ORIENTED_EDGE ( 'NONE', *, *, #1178, .F. ) ;
#20608 = CARTESIAN_POINT ( 'NONE',  ( -3.756430356250003655, -27.95312499938548711, 8.999999999999992895 ) ) ;
#20609 = CARTESIAN_POINT ( 'NONE',  ( 0.5000000000000000000, 0.000000000000000000, 19.50000000000000000 ) ) ;
#20610 =( BOUNDED_CURVE ( )  B_SPLINE_CURVE ( 2, ( #23111, #3213, #7152, #25064, #25441, #1127, #13556, #11322, #5193 ),
 .UNSPECIFIED., .F., .F. ) 
 B_SPLINE_CURVE_WITH_KNOTS ( ( 3, 2, 2, 2, 3 ),
 ( 0.7249999999999999778, 0.7333333333333332815, 0.7500000000000000000, 0.7666666666666667185, 0.7750000000000000222 ),
 .UNSPECIFIED. ) 
 CURVE ( )  GEOMETRIC_REPRESENTATION_ITEM ( )  RATIONAL_B_SPLINE_CURVE ( ( 0.9330127018922194093, 0.9330127018922194093, 1.000000000000000000, 0.8660254037844387076, 1.000000000000000000, 0.8660254037844387076, 1.000000000000000000, 0.9330127018922194093, 0.9330127018922194093 ) ) 
 REPRESENTATION_ITEM ( '' )  );
#20611 = CARTESIAN_POINT ( 'NONE',  ( 1.071796769724498999, 28.00134618820329635, 12.99999999999998757 ) ) ;
#20612 = VECTOR ( 'NONE', #25371, 1000.000000000000000 ) ;
#20613 = LINE ( 'NONE', #2431, #16451 ) ;
#20614 = CARTESIAN_POINT ( 'NONE',  ( 0.000000000000000000, 27.72812499938548925, 13.33755215474602984 ) ) ;
#20615 = AXIS2_PLACEMENT_3D ( 'NONE', #6910, #20904, #2993 ) ;
#20616 = ADVANCED_FACE ( 'NONE', ( #7476 ), #3432, .F. ) ;
#20617 = DIRECTION ( 'NONE',  ( 1.000000000000000000, 0.000000000000000000, 0.000000000000000000 ) ) ;
#20618 = CARTESIAN_POINT ( 'NONE',  ( 0.000000000000000000, 0.000000000000000000, 0.000000000000000000 ) ) ;
#20619 = CARTESIAN_POINT ( 'NONE',  ( -30.53863125411927371, -1.952785157361310198, -6.500000000000000000 ) ) ;
#20620 = CARTESIAN_POINT ( 'NONE',  ( 0.7500000000000001110, 0.000000000000000000, 18.19999999999999929 ) ) ;
#20621 = CARTESIAN_POINT ( 'NONE',  ( 2.451530025009009961, 31.00322564728515218, 1.000000000000000000 ) ) ;
#20622 = CARTESIAN_POINT ( 'NONE',  ( 19.60322238135485762, 18.08747285350274581, 12.99999999999999112 ) ) ;
#20623 = CARTESIAN_POINT ( 'NONE',  ( 18.46426205773553164, 21.12045943569482986, 5.746835883940462963 ) ) ;
#20624 = CARTESIAN_POINT ( 'NONE',  ( 16.34066823992098350, 21.65306299583965455, 11.16877607737301226 ) ) ;
#20625 = DIRECTION ( 'NONE',  ( 1.000000000000000000, 0.000000000000000000, -0.000000000000000000 ) ) ;
#20626 = CYLINDRICAL_SURFACE ( 'NONE', #4210, 4.000000000000000000 ) ;
#20627 = CARTESIAN_POINT ( 'NONE',  ( -1.878215178124995832, 29.00312499938548427, 5.746835883940462963 ) ) ;
#20629 = VERTEX_POINT ( 'NONE', #17936 ) ;
#20628 = DIRECTION ( 'NONE',  ( 0.000000000000000000, -1.000000000000000000, 0.000000000000000000 ) ) ;
#20630 =( GEOMETRIC_REPRESENTATION_CONTEXT ( 3 ) GLOBAL_UNCERTAINTY_ASSIGNED_CONTEXT ( ( #3126 ) ) GLOBAL_UNIT_ASSIGNED_CONTEXT ( ( #6522, #14638, #2996 ) ) REPRESENTATION_CONTEXT ( 'NONE', 'WORKASPACE' ) );
#20631 = CARTESIAN_POINT ( 'NONE',  ( 20.75150184982686596, 15.43910709390805280, 8.999999999999992895 ) ) ;
#20632 = CARTESIAN_POINT ( 'NONE',  ( -1.999999999999998224, -12.46410161513774639, 1.199999999999999734 ) ) ;
#20633 = VERTEX_POINT ( 'NONE', #15989 ) ;
#20634 = CARTESIAN_POINT ( 'NONE',  ( 19.43607991388988765, 24.27856662945500688, -6.500000000000000000 ) ) ;
#20635 = CARTESIAN_POINT ( 'NONE',  ( 2.000000000000000888, 27.11874999877096926, 12.46410161513774817 ) ) ;
#20636 = CARTESIAN_POINT ( 'NONE',  ( -3.756430356250004099, -26.97812499938548569, 6.831223922626973533 ) ) ;
#20638 = ORIENTED_EDGE ( 'NONE', *, *, #7993, .F. ) ;
#20637 = CYLINDRICAL_SURFACE ( 'NONE', #20865, 4.000000000000000000 ) ;
#20639 = DIRECTION ( 'NONE',  ( 0.000000000000000000, 0.000000000000000000, 1.000000000000000000 ) ) ;
#20640 = ORIENTED_EDGE ( 'NONE', *, *, #5876, .T. ) ;
#20641 = CARTESIAN_POINT ( 'NONE',  ( 1.878215178124998497, -29.60312499938548569, 12.25316411605951927 ) ) ;
#20642 = ORIENTED_EDGE ( 'NONE', *, *, #20801, .T. ) ;
#20643 = APPLICATION_CONTEXT ( 'automotive_design' ) ;
#20644 = ORIENTED_EDGE ( 'NONE', *, *, #10150, .F. ) ;
#20645 = CARTESIAN_POINT ( 'NONE',  ( -7.248980000274416469, -30.24338421796776544, 1.000000000000000000 ) ) ;
#20646 = CARTESIAN_POINT ( 'NONE',  ( -3.849711841530632839, 38.61087488181074434, 13.45662818444764497 ) ) ;
#20647 = CYLINDRICAL_SURFACE ( 'NONE', #6004, 0.5000000000000002220 ) ;
#20648 = ADVANCED_FACE ( 'NONE', ( #13374 ), #3674, .F. ) ;
#20649 = EDGE_CURVE ( 'NONE', #7097, #14349, #11625, .T. ) ;
#20650 = CARTESIAN_POINT ( 'NONE',  ( -1.878215178124995832, -5.746835883940462963, 2.653124999385483740 ) ) ;
#20651 = CARTESIAN_POINT ( 'NONE',  ( -1.071796769724492338, -27.10134618820329777, 12.99999999999999467 ) ) ;
#20652 = CARTESIAN_POINT ( 'NONE',  ( 3.756430356250002323, 29.15312499938548640, 11.16877607737301226 ) ) ;
#20653 = ADVANCED_FACE ( 'NONE', ( #19497 ), #9445, .F. ) ;
#20654 = CARTESIAN_POINT ( 'NONE',  ( 4.000000000000003553, -8.999999999999992895, 1.743749998770967924 ) ) ;
#20655 = CARTESIAN_POINT ( 'NONE',  ( 1.999999999999995781, -28.75000000000000000, 5.535898384862237620 ) ) ;
#20656 = UNCERTAINTY_MEASURE_WITH_UNIT (LENGTH_MEASURE( 1.000000000000000082E-05 ), #24180, 'distance_accuracy_value', 'NONE');
#20657 = CARTESIAN_POINT ( 'NONE',  ( 1.878215178125000939, 27.76562499938548356, 12.25316411605952283 ) ) ;
#20658 = DIRECTION ( 'NONE',  ( -0.000000000000000000, -0.000000000000000000, 1.000000000000000000 ) ) ;
#20659 = DIRECTION ( 'NONE',  ( -0.000000000000000000, -0.000000000000000000, 1.000000000000000000 ) ) ;
#20660 = CYLINDRICAL_SURFACE ( 'NONE', #21394, 0.5000000000000004441 ) ;
#20661 = EDGE_CURVE ( 'NONE', #8766, #6385, #19629, .T. ) ;
#20662 = CARTESIAN_POINT ( 'NONE',  ( -3.756430356250003655, -26.60312499938548569, 8.999999999999992895 ) ) ;
#20663 = CYLINDRICAL_SURFACE ( 'NONE', #18601, 0.5000000000000004441 ) ;
#20664 = CARTESIAN_POINT ( 'NONE',  ( 4.000000000000003553, 27.64374999877096784, 8.999999999999992895 ) ) ;
#20665 = CARTESIAN_POINT ( 'NONE',  ( 0.000000000000000000, 0.000000000000000000, 1.000000000000000000 ) ) ;
#20666 = DIRECTION ( 'NONE',  ( 1.000000000000000000, 0.000000000000000000, 0.000000000000000000 ) ) ;
#20667 = ORIENTED_EDGE ( 'NONE', *, *, #7657, .T. ) ;
#20668 = EDGE_CURVE ( 'NONE', #11918, #14407, #9123, .T. ) ;
#20669 = DIRECTION ( 'NONE',  ( 0.000000000000000000, -1.000000000000000000, 0.000000000000000000 ) ) ;
#20671 = ORIENTED_EDGE ( 'NONE', *, *, #19751, .F. ) ;
#20670 = DIRECTION ( 'NONE',  ( 0.000000000000000000, 0.000000000000000000, -1.000000000000000000 ) ) ;
#20672 = ORIENTED_EDGE ( 'NONE', *, *, #22411, .F. ) ;
#20673 = VERTEX_POINT ( 'NONE', #9565 ) ;
#20674 = ORIENTED_EDGE ( 'NONE', *, *, #18146, .T. ) ;
#20675 = ORIENTED_EDGE ( 'NONE', *, *, #20254, .T. ) ;
#20676 = CARTESIAN_POINT ( 'NONE',  ( -30.63887302793249034, -5.335677986744600254, 1.000000000000000000 ) ) ;
#20677 = ORIENTED_EDGE ( 'NONE', *, *, #3735, .T. ) ;
#20678 = FACE_OUTER_BOUND ( 'NONE', #2340, .T. ) ;
#20679 = CARTESIAN_POINT ( 'NONE',  ( -3.756430356249996105, 28.59062499938548640, 6.831223922626973533 ) ) ;
#20680 = CARTESIAN_POINT ( 'NONE',  ( 3.756430356250002323, -11.16877607737301226, 2.465624999385482852 ) ) ;
#20681 = CARTESIAN_POINT ( 'NONE',  ( 3.401318489840878367, -30.91344420362549528, -2.750000000000000000 ) ) ;
#20682 = CARTESIAN_POINT ( 'NONE',  ( 21.91595456452976975, 19.25975718657032232, 12.25316411605952283 ) ) ;
#20683 = CARTESIAN_POINT ( 'NONE',  ( 0.000000000000000000, 0.000000000000000000, 15.00000000000000178 ) ) ;
#20684 = DIRECTION ( 'NONE',  ( 0.000000000000000000, 0.000000000000000000, 1.000000000000000000 ) ) ;
#20685 = AXIS2_PLACEMENT_3D ( 'NONE', #10836, #7432, #17269 ) ;
#20686 = CARTESIAN_POINT ( 'NONE',  ( -1.878215178124998497, -12.25316411605951927, 4.040624999385483918 ) ) ;
#20687 = PRODUCT_RELATED_PRODUCT_CATEGORY ( 'part', '', ( #20064 ) ) ;
#20688 = CARTESIAN_POINT ( 'NONE',  ( 13.24173596767378847, 28.14012133169319796, 1.000000000000000000 ) ) ;
#20689 = CARTESIAN_POINT ( 'NONE',  ( -3.999999999999995559, 27.83124999877096784, 6.690598923241487306 ) ) ;
#20690 = DIRECTION ( 'NONE',  ( 0.000000000000000000, 0.000000000000000000, 1.000000000000000000 ) ) ;
#20691 = DIRECTION ( 'NONE',  ( 1.000000000000000000, 0.000000000000000000, 0.000000000000000000 ) ) ;
#20692 = CARTESIAN_POINT ( 'NONE',  ( -3.756430356249997438, -11.16877607737301048, 2.765624999385486227 ) ) ;
#20693 = CYLINDRICAL_SURFACE ( 'NONE', #18295, 4.000000000000000000 ) ;
#20694 = DIRECTION ( 'NONE',  ( 0.000000000000000000, 0.000000000000000000, 1.000000000000000000 ) ) ;
#20695 = ORIENTED_EDGE ( 'NONE', *, *, #5845, .F. ) ;
#20696 = EDGE_CURVE ( 'NONE', #14918, #22793, #13782, .T. ) ;
#20697 = ORIENTED_EDGE ( 'NONE', *, *, #9037, .F. ) ;
#20698 = CARTESIAN_POINT ( 'NONE',  ( 3.756430356250004543, 27.54062499938548925, 6.831223922626973533 ) ) ;
#20699 = EDGE_CURVE ( 'NONE', #14520, #5668, #1734, .T. ) ;
#20700 = ORIENTED_EDGE ( 'NONE', *, *, #202, .T. ) ;
#20701 = DIRECTION ( 'NONE',  ( 0.000000000000000000, 0.000000000000000000, 1.000000000000000000 ) ) ;
#20702 = EDGE_LOOP ( 'NONE', ( #19470, #15952, #22892, #4007 ) ) ;
#20703 = AXIS2_PLACEMENT_3D ( 'NONE', #7508, #25689, #17587 ) ;
#20704 = CARTESIAN_POINT ( 'NONE',  ( -5.840899737312954976, 34.50000000000000000, 10.37254881831481512 ) ) ;
#20705 = EDGE_LOOP ( 'NONE', ( #1983, #2109, #15357, #93 ) ) ;
#20706 = CARTESIAN_POINT ( 'NONE',  ( 23.96650046397252609, 18.30964621448006824, 8.999999999999992895 ) ) ;
#20707 = ORIENTED_EDGE ( 'NONE', *, *, #18886, .F. ) ;
#20708 = CIRCLE ( 'NONE', #14030, 31.10000000000000142 ) ;
#20709 = DIRECTION ( 'NONE',  ( 0.000000000000000000, 0.000000000000000000, 1.000000000000000000 ) ) ;
#20710 = CARTESIAN_POINT ( 'NONE',  ( 2.000000000000003997, 25.97500000000000142, 5.535898384862238508 ) ) ;
#20711 = CARTESIAN_POINT ( 'NONE',  ( -1.071796769724487230, 28.22634618820330132, 4.999999999999992006 ) ) ;
#20712 = DIRECTION ( 'NONE',  ( -0.3090169943749382919, 0.9510565162951566398, 0.000000000000000000 ) ) ;
#20713 = CARTESIAN_POINT ( 'NONE',  ( 22.07732706455164617, 16.76493230863282591, 11.16877607737301226 ) ) ;
#20714 =( BOUNDED_CURVE ( )  B_SPLINE_CURVE ( 2, ( #19910, #25685, #1768, #11823, #7766, #11553, #5937, #11434, #3975 ),
 .UNSPECIFIED., .F., .F. ) 
 B_SPLINE_CURVE_WITH_KNOTS ( ( 3, 2, 2, 2, 3 ),
 ( 0.02500000000000000486, 0.03333333333333333287, 0.05000000000000000278, 0.06666666666666666574, 0.07500000000000001110 ),
 .UNSPECIFIED. ) 
 CURVE ( )  GEOMETRIC_REPRESENTATION_ITEM ( )  RATIONAL_B_SPLINE_CURVE ( ( 0.9330127018922194093, 0.9330127018922194093, 1.000000000000000000, 0.8660254037844387076, 1.000000000000000000, 0.8660254037844387076, 1.000000000000000000, 0.9330127018922191873, 0.9330127018922192983 ) ) 
 REPRESENTATION_ITEM ( '' )  );
#20715 = VECTOR ( 'NONE', #1704, 1000.000000000000000 ) ;
#20716 = CARTESIAN_POINT ( 'NONE',  ( -1.878215178124998497, 29.04062499938548569, 12.25316411605951927 ) ) ;
#20717 = CARTESIAN_POINT ( 'NONE',  ( 15.33304107673014904, 20.64543583264882898, 6.831223922626973533 ) ) ;
#20718 = CARTESIAN_POINT ( 'NONE',  ( -21.65113613650310143, 22.32573188046944068, 1.000000000000000000 ) ) ;
#20719 = ADVANCED_FACE ( 'NONE', ( #21864 ), #17689, .T. ) ;
#20720 = ORIENTED_EDGE ( 'NONE', *, *, #15130, .T. ) ;
#20721 = DIRECTION ( 'NONE',  ( 1.000000000000000000, 0.000000000000000000, 0.000000000000000000 ) ) ;
#20722 = PRODUCT_DEFINITION_SHAPE ( 'NONE', 'NONE',  #25879 ) ;
#20723 = CARTESIAN_POINT ( 'NONE',  ( 2.000000000000003553, 26.36874999877097281, 5.535898384862238508 ) ) ;
#20724 = CARTESIAN_POINT ( 'NONE',  ( 0.000000000000000000, 0.000000000000000000, 17.69999999999999929 ) ) ;
#20726 = ADVANCED_FACE ( 'NONE', ( #23684 ), #21480, .T. ) ;
#20725 = CARTESIAN_POINT ( 'NONE',  ( -3.756430356250002323, -27.80312499938548143, 11.16877607737301403 ) ) ;
#20727 = CARTESIAN_POINT ( 'NONE',  ( -29.62293631110035363, 7.734255490827311341, -6.500000000000000000 ) ) ;
#20728 = CARTESIAN_POINT ( 'NONE',  ( 4.000000000000003553, 28.99374999877096926, 8.999999999999992895 ) ) ;
#20729 = DIRECTION ( 'NONE',  ( 0.000000000000000000, -1.000000000000000000, 0.000000000000000000 ) ) ;
#20731 = EDGE_LOOP ( 'NONE', ( #9596, #16918, #8218, #22733 ) ) ;
#20730 = CARTESIAN_POINT ( 'NONE',  ( -3.756430356249996549, 29.52812499938548996, 8.999999999999992895 ) ) ;
#20732 = VERTEX_POINT ( 'NONE', #7613 ) ;
#20733 = CARTESIAN_POINT ( 'NONE',  ( -1.999999999999998224, 28.84374999877096712, 12.46410161513774639 ) ) ;
#20734 = CYLINDRICAL_SURFACE ( 'NONE', #10055, 4.000000000000000000 ) ;
#20735 = VERTEX_POINT ( 'NONE', #9948 ) ;
#20736 = EDGE_CURVE ( 'NONE', #1055, #2880, #2438, .T. ) ;
#20737 = CARTESIAN_POINT ( 'NONE',  ( -3.756430356250002323, -26.11562499938548498, 11.16877607737301403 ) ) ;
#20738 = DIRECTION ( 'NONE',  ( 0.000000000000000000, 0.000000000000000000, -1.000000000000000000 ) ) ;
#20739 = CARTESIAN_POINT ( 'NONE',  ( 6.009258394948636914E-15, 26.60312499938547859, 4.662447845253954171 ) ) ;
#20740 = ADVANCED_FACE ( 'NONE', ( #8001 ), #13511, .F. ) ;
#20741 = CARTESIAN_POINT ( 'NONE',  ( 1.071796769724494114, 26.25759618943234130, 12.99999999999999112 ) ) ;
#20742 = CARTESIAN_POINT ( 'NONE',  ( 4.006172263299091013E-15, 25.11250000000000426, 4.381197846482986158 ) ) ;
#20743 = DIRECTION ( 'NONE',  ( 0.000000000000000000, 0.000000000000000000, 1.000000000000000000 ) ) ;
#20744 = DIRECTION ( 'NONE',  ( 0.000000000000000000, 0.000000000000000000, -1.000000000000000000 ) ) ;
#20745 = DIRECTION ( 'NONE',  ( 1.000000000000000000, 0.000000000000000000, 0.000000000000000000 ) ) ;
#20746 = DIRECTION ( 'NONE',  ( 0.000000000000000000, 0.000000000000000000, 1.000000000000000000 ) ) ;
#20747 = DIRECTION ( 'NONE',  ( 1.000000000000000000, 0.000000000000000000, 0.000000000000000000 ) ) ;
#20748 = CARTESIAN_POINT ( 'NONE',  ( 19.30843454290614147, 19.30843454290607752, 4.999999999999991118 ) ) ;
#20749 = DIRECTION ( 'NONE',  ( -0.000000000000000000, -0.000000000000000000, 1.000000000000000000 ) ) ;
#20750 = CARTESIAN_POINT ( 'NONE',  ( 22.63417365473605614, 17.32177889881723587, 11.16877607737301226 ) ) ;
#20751 = CARTESIAN_POINT ( 'NONE',  ( 15.65123912826409480, 20.96363388418277296, 6.831223922626973533 ) ) ;
#20752 = DIRECTION ( 'NONE',  ( 0.000000000000000000, 0.000000000000000000, 1.000000000000000000 ) ) ;
#20753 = EDGE_CURVE ( 'NONE', #9464, #161, #21729, .T. ) ;
#20754 = CYLINDRICAL_SURFACE ( 'NONE', #19663, 0.5000000000000004441 ) ;
#20755 = CARTESIAN_POINT ( 'NONE',  ( -3.756430356249995661, 27.57812499938548356, 6.831223922626973533 ) ) ;
#20756 = CARTESIAN_POINT ( 'NONE',  ( 3.000000000000003997, -8.999999999999992895, 0.000000000000000000 ) ) ;
#20757 = CARTESIAN_POINT ( 'NONE',  ( 20.64530830152148155, 14.98845405202903613, 8.999999999999992895 ) ) ;
#20758 = LINE ( 'NONE', #14754, #16300 ) ;
#20759 = ORIENTED_EDGE ( 'NONE', *, *, #14187, .T. ) ;
#20760 = DIRECTION ( 'NONE',  ( 1.000000000000000000, 0.000000000000000000, -0.000000000000000000 ) ) ;
#20761 = CARTESIAN_POINT ( 'NONE',  ( 2.000000000000003997, 27.71874999877097068, 5.535898384862238508 ) ) ;
#20762 = CARTESIAN_POINT ( 'NONE',  ( 3.756430356249995661, -28.02812499938548640, 6.831223922626973533 ) ) ;
#20764 = ORIENTED_EDGE ( 'NONE', *, *, #12864, .F. ) ;
#20763 = CARTESIAN_POINT ( 'NONE',  ( -1.071796769724487230, 25.71115380933864003, 12.99999999999999467 ) ) ;
#20765 = CARTESIAN_POINT ( 'NONE',  ( 1.071796769724489895, 29.80134618820331127, 12.99999999999999467 ) ) ;
#20766 =( BOUNDED_SURFACE ( )  B_SPLINE_SURFACE ( 1, 2, ( 
 ( #7290, #13297, #21271, #11461, #15149, #1525, #3354, #17097, #23495, #19312, #1407, #17361, #5582, #25586, #5699, #11579, #1793, #19551, #1654, #9630, #7406, #15385, #7670, #13678, #21651, #3733, #11717, #13178, #23117, #21148, #21916, #17865, #334, #18251, #2300, #13947, #6348, #24261, #13813, #23880, #21792, #3874, #24005, #14070, #15907, #18140, #10007, #5965, #90, #22174, #12233, #5827, #6086, #20200, #8308, #22036, #7920, #16044, #2039, #3997, #11964, #12098, #11846, #12359, #4259, #19935, #25711, #23740, #22303, #14341, #4119, #10257, #19817, #16294, #4380, #20325, #9761, #20074, #2176, #18001, #1918, #17740, #7792, #8061, #15771, #9879, #25837, #10137, #214, #8184, #16162, #24125, #6211, #14201, #10907, #8690, #20728, #20599, #8967, #10377, #986, #851, #22564, #4504, #2942, #18903, #16942, #8446, #14583, #24911, #6867, #22822, #6596, #22949, #4646, #6987, #16555, #12628, #2415, #10523, #8832 ),
 ( #14971, #6732, #14724, #5033, #6475, #477, #8574, #14850, #24645, #2806, #4899, #18377, #20455, #24399, #12481, #13016, #12876, #10770, #16435, #2554, #14461, #2685, #16677, #22423, #723, #18520, #18761, #607, #24514, #16820, #10646, #24785, #22702, #18640, #4782, #12756, #20852, #19021, #3582, #7377, #7125, #9216, #17206, #23594, #25177, #19142, #19406, #15112, #11160, #1621, #11040, #25037, #21238, #9594, #1233, #17063, #3459, #7259, #1376, #13149, #1104, #25558, #23086, #7640, #21113, #9079, #19277, #5172, #3192, #15238, #15354, #15627, #23203, #5287, #19520, #21503, #5673, #13264, #20996, #11433, #5418, #15496, #3320, #17581, #11552, #3074, #11295, #9352, #1497, #13402, #23464, #17333, #25299, #23327, #21379, #9470, #17447, #25415, #7504, #5552, #13536, #11939, #19909, #9855, #6183, #2008, #15877, #5936, #24101, #1767, #7888, #19659, #25684, #3843, #14172, #13652, #6063, #16140, #17970, #21891, #4090 ) ),
 .UNSPECIFIED., .F., .F., .F. ) 
 B_SPLINE_SURFACE_WITH_KNOTS ( ( 2, 2 ),
 ( 3, 2, 2, 2, 2, 2, 2, 2, 2, 2, 2, 2, 2, 2, 2, 2, 2, 2, 2, 2, 2, 2, 2, 2, 2, 2, 2, 2, 2, 2, 2, 2, 2, 2, 2, 2, 2, 2, 2, 2, 2, 2, 2, 2, 2, 2, 2, 2, 2, 2, 2, 2, 2, 2, 2, 2, 2, 2, 2, 2, 3 ),
 ( 0.000000000000000000, 1.000000000000000000 ),
 ( 0.000000000000000000, 0.01666666666666666644, 0.03333333333333333287, 0.05000000000000000278, 0.06666666666666666574, 0.08333333333333332871, 0.1000000000000000056, 0.1166666666666666685, 0.1333333333333333315, 0.1499999999999999944, 0.1666666666666666574, 0.1833333333333333204, 0.2000000000000000111, 0.2166666666666666741, 0.2333333333333333370, 0.2500000000000000000, 0.2666666666666666630, 0.2833333333333333259, 0.2999999999999999889, 0.3166666666666666519, 0.3333333333333333148, 0.3499999999999999778, 0.3666666666666666408, 0.3833333333333333592, 0.4000000000000000222, 0.4166666666666666852, 0.4333333333333333481, 0.4500000000000000111, 0.4666666666666666741, 0.4833333333333333370, 0.5000000000000000000, 0.5166666666666667185, 0.5333333333333333259, 0.5500000000000000444, 0.5666666666666666519, 0.5833333333333333703, 0.5999999999999999778, 0.6166666666666666963, 0.6333333333333333037, 0.6500000000000000222, 0.6666666666666666297, 0.6833333333333333481, 0.6999999999999999556, 0.7166666666666666741, 0.7333333333333332815, 0.7500000000000000000, 0.7666666666666667185, 0.7833333333333333259, 0.8000000000000000444, 0.8166666666666666519, 0.8333333333333333703, 0.8499999999999999778, 0.8666666666666666963, 0.8833333333333333037, 0.9000000000000000222, 0.9166666666666666297, 0.9333333333333333481, 0.9499999999999999556, 0.9666666666666666741, 0.9833333333333332815, 1.000000000000000000 ),
 .UNSPECIFIED. ) 
 GEOMETRIC_REPRESENTATION_ITEM ( )  RATIONAL_B_SPLINE_SURFACE ( (
 ( 1.000000000000000000, 0.8660254037844387076, 1.000000000000000000, 0.8660254037844387076, 1.000000000000000000, 0.8660254037844387076, 1.000000000000000000, 0.8660254037844387076, 1.000000000000000000, 0.8660254037844387076, 1.000000000000000000, 0.8660254037844387076, 1.000000000000000000, 0.8660254037844387076, 1.000000000000000000, 0.8660254037844387076, 1.000000000000000000, 0.8660254037844387076, 1.000000000000000000, 0.8660254037844387076, 1.000000000000000000, 0.8660254037844387076, 1.000000000000000000, 0.8660254037844387076, 1.000000000000000000, 0.8660254037844387076, 1.000000000000000000, 0.8660254037844387076, 1.000000000000000000, 0.8660254037844387076, 1.000000000000000000, 0.8660254037844387076, 1.000000000000000000, 0.8660254037844387076, 1.000000000000000000, 0.8660254037844387076, 1.000000000000000000, 0.8660254037844387076, 1.000000000000000000, 0.8660254037844387076, 1.000000000000000000, 0.8660254037844387076, 1.000000000000000000, 0.8660254037844387076, 1.000000000000000000, 0.8660254037844387076, 1.000000000000000000, 0.8660254037844387076, 1.000000000000000000, 0.8660254037844387076, 1.000000000000000000, 0.8660254037844387076, 1.000000000000000000, 0.8660254037844387076, 1.000000000000000000, 0.8660254037844387076, 1.000000000000000000, 0.8660254037844387076, 1.000000000000000000, 0.8660254037844387076, 1.000000000000000000, 0.8660254037844387076, 1.000000000000000000, 0.8660254037844387076, 1.000000000000000000, 0.8660254037844387076, 1.000000000000000000, 0.8660254037844387076, 1.000000000000000000, 0.8660254037844387076, 1.000000000000000000, 0.8660254037844387076, 1.000000000000000000, 0.8660254037844387076, 1.000000000000000000, 0.8660254037844387076, 1.000000000000000000, 0.8660254037844387076, 1.000000000000000000, 0.8660254037844387076, 1.000000000000000000, 0.8660254037844387076, 1.000000000000000000, 0.8660254037844387076, 1.000000000000000000, 0.8660254037844387076, 1.000000000000000000, 0.8660254037844387076, 1.000000000000000000, 0.8660254037844387076, 1.000000000000000000, 0.8660254037844387076, 1.000000000000000000, 0.8660254037844387076, 1.000000000000000000, 0.8660254037844387076, 1.000000000000000000, 0.8660254037844387076, 1.000000000000000000, 0.8660254037844387076, 1.000000000000000000, 0.8660254037844387076, 1.000000000000000000, 0.8660254037844387076, 1.000000000000000000, 0.8660254037844387076, 1.000000000000000000, 0.8660254037844387076, 1.000000000000000000, 0.8660254037844387076, 1.000000000000000000, 0.8660254037844387076, 1.000000000000000000, 0.8660254037844387076, 1.000000000000000000, 0.8660254037844387076, 1.000000000000000000, 0.8660254037844387076, 1.000000000000000000, 0.8660254037844387076, 1.000000000000000000),
 ( 1.000000000000000000, 0.8660254037844387076, 1.000000000000000000, 0.8660254037844387076, 1.000000000000000000, 0.8660254037844387076, 1.000000000000000000, 0.8660254037844387076, 1.000000000000000000, 0.8660254037844387076, 1.000000000000000000, 0.8660254037844387076, 1.000000000000000000, 0.8660254037844387076, 1.000000000000000000, 0.8660254037844387076, 1.000000000000000000, 0.8660254037844387076, 1.000000000000000000, 0.8660254037844387076, 1.000000000000000000, 0.8660254037844387076, 1.000000000000000000, 0.8660254037844387076, 1.000000000000000000, 0.8660254037844387076, 1.000000000000000000, 0.8660254037844387076, 1.000000000000000000, 0.8660254037844387076, 1.000000000000000000, 0.8660254037844387076, 1.000000000000000000, 0.8660254037844387076, 1.000000000000000000, 0.8660254037844387076, 1.000000000000000000, 0.8660254037844387076, 1.000000000000000000, 0.8660254037844387076, 1.000000000000000000, 0.8660254037844387076, 1.000000000000000000, 0.8660254037844387076, 1.000000000000000000, 0.8660254037844387076, 1.000000000000000000, 0.8660254037844387076, 1.000000000000000000, 0.8660254037844387076, 1.000000000000000000, 0.8660254037844387076, 1.000000000000000000, 0.8660254037844387076, 1.000000000000000000, 0.8660254037844387076, 1.000000000000000000, 0.8660254037844387076, 1.000000000000000000, 0.8660254037844387076, 1.000000000000000000, 0.8660254037844387076, 1.000000000000000000, 0.8660254037844387076, 1.000000000000000000, 0.8660254037844387076, 1.000000000000000000, 0.8660254037844387076, 1.000000000000000000, 0.8660254037844387076, 1.000000000000000000, 0.8660254037844387076, 1.000000000000000000, 0.8660254037844387076, 1.000000000000000000, 0.8660254037844387076, 1.000000000000000000, 0.8660254037844387076, 1.000000000000000000, 0.8660254037844387076, 1.000000000000000000, 0.8660254037844387076, 1.000000000000000000, 0.8660254037844387076, 1.000000000000000000, 0.8660254037844387076, 1.000000000000000000, 0.8660254037844387076, 1.000000000000000000, 0.8660254037844387076, 1.000000000000000000, 0.8660254037844387076, 1.000000000000000000, 0.8660254037844387076, 1.000000000000000000, 0.8660254037844387076, 1.000000000000000000, 0.8660254037844387076, 1.000000000000000000, 0.8660254037844387076, 1.000000000000000000, 0.8660254037844387076, 1.000000000000000000, 0.8660254037844387076, 1.000000000000000000, 0.8660254037844387076, 1.000000000000000000, 0.8660254037844387076, 1.000000000000000000, 0.8660254037844387076, 1.000000000000000000, 0.8660254037844387076, 1.000000000000000000, 0.8660254037844387076, 1.000000000000000000, 0.8660254037844387076, 1.000000000000000000, 0.8660254037844387076, 1.000000000000000000, 0.8660254037844387076, 1.000000000000000000) ) ) 
 REPRESENTATION_ITEM ( '' )  SURFACE ( )  );
#20767 = EDGE_CURVE ( 'NONE', #21696, #16617, #24581, .T. ) ;
#20768 = ORIENTED_EDGE ( 'NONE', *, *, #13212, .T. ) ;
#20769 = CARTESIAN_POINT ( 'NONE',  ( -3.735045420075836212E-15, -29.41562499938548569, 4.662447845253954171 ) ) ;
#20770 = ORIENTED_EDGE ( 'NONE', *, *, #4364, .F. ) ;
#20771 = ORIENTED_EDGE ( 'NONE', *, *, #9258, .F. ) ;
#20772 = CARTESIAN_POINT ( 'NONE',  ( 14.54246377227351061, -27.49048467073857793, 1.000000000000000000 ) ) ;
#20773 = CARTESIAN_POINT ( 'NONE',  ( 3.756430356250006319, 27.99062499938548854, 6.831223922626973533 ) ) ;
#20774 = EDGE_CURVE ( 'NONE', #1602, #17557, #9826, .T. ) ;
#20775 = CARTESIAN_POINT ( 'NONE',  ( 2.000000000000003997, -5.535898384862238508, 1.875000000000001776 ) ) ;
#20776 = CARTESIAN_POINT ( 'NONE',  ( -1.878215178124995832, -5.746835883940462963, 1.303124999385483429 ) ) ;
#20777 = CARTESIAN_POINT ( 'NONE',  ( -4.000000000000003553, -27.23124999877096641, 6.690598923241489970 ) ) ;
#20778 = CARTESIAN_POINT ( 'NONE',  ( 2.672651547586948120E-15, 27.27812499938548285, 13.33755215474602984 ) ) ;
#20779 = CARTESIAN_POINT ( 'NONE',  ( 16.89101323559370016, 22.54786748508600525, 6.690598923241487306 ) ) ;
#20780 = CARTESIAN_POINT ( 'NONE',  ( 3.918623196469491088, 34.50000000000000000, 13.54361004533742907 ) ) ;
#20781 = CARTESIAN_POINT ( 'NONE',  ( -3.756430356249997438, 28.10312499938548569, 11.16877607737301048 ) ) ;
#20782 = CARTESIAN_POINT ( 'NONE',  ( 3.756430356250003655, -8.999999999999992895, 4.696874999385483918 ) ) ;
#20783 = CARTESIAN_POINT ( 'NONE',  ( 21.61951122846571138, 20.80093850620003337, 12.96878440844335678 ) ) ;
#20784 = CARTESIAN_POINT ( 'NONE',  ( 31.10000000000000142, -1.085850696380214537E-13, 1.000000000000000000 ) ) ;
#20785 = CARTESIAN_POINT ( 'NONE',  ( 3.756430356249996994, -25.92812499938548498, 8.999999999999992895 ) ) ;
#20786 = CARTESIAN_POINT ( 'NONE',  ( 3.756430356250004099, 25.74062499938548143, 6.831223922626973533 ) ) ;
#20787 = DIRECTION ( 'NONE',  ( 0.000000000000000000, 0.000000000000000000, -1.000000000000000000 ) ) ;
#20788 = CARTESIAN_POINT ( 'NONE',  ( -4.000000000000003553, -28.63749999999999929, 6.690598923241489970 ) ) ;
#20789 =( REPRESENTATION_RELATIONSHIP ('NONE','NONE', #25031, #16033 ) REPRESENTATION_RELATIONSHIP_WITH_TRANSFORMATION ( #25055 )SHAPE_REPRESENTATION_RELATIONSHIP( ) );
#20790 = ORIENTED_EDGE ( 'NONE', *, *, #12495, .T. ) ;
#20791 = DIRECTION ( 'NONE',  ( 0.000000000000000000, 0.000000000000000000, 1.000000000000000000 ) ) ;
#20793 = ORIENTED_EDGE ( 'NONE', *, *, #17195, .F. ) ;
#20792 = CARTESIAN_POINT ( 'NONE',  ( 3.469446951953614189E-15, 40.00000000000000000, 8.999999999999992895 ) ) ;
#20795 = ORIENTED_EDGE ( 'NONE', *, *, #14808, .F. ) ;
#20794 = EDGE_CURVE ( 'NONE', #25495, #12364, #19980, .T. ) ;
#20796 = CIRCLE ( 'NONE', #802, 0.5000000000000002220 ) ;
#20797 = VERTEX_POINT ( 'NONE', #10684 ) ;
#20798 = VERTEX_POINT ( 'NONE', #8609 ) ;
#20799 = ORIENTED_EDGE ( 'NONE', *, *, #2796, .F. ) ;
#20800 = DIRECTION ( 'NONE',  ( 0.000000000000000000, -1.000000000000000000, 0.000000000000000000 ) ) ;
#20801 = EDGE_CURVE ( 'NONE', #19820, #14690, #12793, .T. ) ;
#20803 = ORIENTED_EDGE ( 'NONE', *, *, #16538, .F. ) ;
#20802 = CIRCLE ( 'NONE', #21224, 4.000000000000000000 ) ;
#20804 = FACE_OUTER_BOUND ( 'NONE', #11465, .T. ) ;
#20805 = CARTESIAN_POINT ( 'NONE',  ( -3.756430356249997438, 29.56562499938549493, 11.16877607737301048 ) ) ;
#20806 = CARTESIAN_POINT ( 'NONE',  ( -3.756430356249997882, -11.16877607737301226, 4.115624999385481431 ) ) ;
#20807 = CARTESIAN_POINT ( 'NONE',  ( 2.000000000000000888, 29.42500000000000071, 12.46410161513774817 ) ) ;
#20808 = EDGE_CURVE ( 'NONE', #4579, #9527, #8765, .T. ) ;
#20809 = CARTESIAN_POINT ( 'NONE',  ( 1.878215178125004048, 26.22812499938548569, 5.746835883940462963 ) ) ;
#20810 = CARTESIAN_POINT ( 'NONE',  ( -15.85973458909327150, -20.67279826512042362, 20.00001200000000168 ) ) ;
#20811 = AXIS2_PLACEMENT_3D ( 'NONE', #24093, #22134, #10487 ) ;
#20812 = CARTESIAN_POINT ( 'NONE',  ( 2.000000000000000888, -12.46410161513774817, 0.3750000000000003331 ) ) ;
#20813 = DIRECTION ( 'NONE',  ( -0.7071067811865487940, -0.7071067811865463515, 0.000000000000000000 ) ) ;
#20814 = FACE_OUTER_BOUND ( 'NONE', #13239, .T. ) ;
#20815 = CARTESIAN_POINT ( 'NONE',  ( 0.000000000000000000, 0.000000000000000000, -6.500000000000000000 ) ) ;
#20816 = CARTESIAN_POINT ( 'NONE',  ( -1.499999999999998224, -7.499999999999992895, 4.999999999999993783 ) ) ;
#20817 = CARTESIAN_POINT ( 'NONE',  ( -3.756430356249997438, -11.16877607737301048, 1.865624999385482985 ) ) ;
#20818 = CARTESIAN_POINT ( 'NONE',  ( -27.10000000000000497, -0.5999999999999998668, 19.59999999999999787 ) ) ;
#20819 = CARTESIAN_POINT ( 'NONE',  ( 21.21320343559646915, 21.21320343559638744, 8.999999999999992895 ) ) ;
#20820 = ORIENTED_EDGE ( 'NONE', *, *, #13948, .F. ) ;
#20821 = EDGE_CURVE ( 'NONE', #13301, #20277, #14991, .T. ) ;
#20822 = ORIENTED_EDGE ( 'NONE', *, *, #11699, .T. ) ;
#20823 = ORIENTED_EDGE ( 'NONE', *, *, #15704, .F. ) ;
#20824 = DIRECTION ( 'NONE',  ( 1.000000000000000000, 0.000000000000000000, -0.000000000000000000 ) ) ;
#20825 = ORIENTED_EDGE ( 'NONE', *, *, #4892, .F. ) ;
#20826 = CARTESIAN_POINT ( 'NONE',  ( 1.878215178124995832, -26.30312499938548498, 5.746835883940462963 ) ) ;
#20827 = ORIENTED_EDGE ( 'NONE', *, *, #17605, .F. ) ;
#20828 = CYLINDRICAL_SURFACE ( 'NONE', #3404, 4.000000000000000000 ) ;
#20829 = EDGE_LOOP ( 'NONE', ( #7299, #19284, #5676, #9878 ) ) ;
#20830 = AXIS2_PLACEMENT_3D ( 'NONE', #23140, #5340, #5219 ) ;
#20831 = CARTESIAN_POINT ( 'NONE',  ( 0.000000000000000000, 0.000000000000000000, 18.19999999999999929 ) ) ;
#20832 = ADVANCED_FACE ( 'NONE', ( #6034 ), #2601, .F. ) ;
#20833 = CARTESIAN_POINT ( 'NONE',  ( 4.000000000000003553, 25.44999999999999929, 8.999999999999992895 ) ) ;
#20834 = CARTESIAN_POINT ( 'NONE',  ( 1.626862140677534194E-14, 28.43124999877096570, 12.99999999999999289 ) ) ;
#20835 = AXIS2_PLACEMENT_3D ( 'NONE', #5177, #21117, #17211 ) ;
#20836 = CIRCLE ( 'NONE', #19549, 4.000000000000000000 ) ;
#20837 = DIRECTION ( 'NONE',  ( 1.000000000000000000, 0.000000000000000000, -0.000000000000000000 ) ) ;
#20838 = CARTESIAN_POINT ( 'NONE',  ( -3.999999999999997335, 28.35624999877096997, 11.30940107675849404 ) ) ;
#20839 = CARTESIAN_POINT ( 'NONE',  ( 20.72271187127746828, 18.06651449331802439, 12.25316411605952283 ) ) ;
#20840 = EDGE_CURVE ( 'NONE', #12137, #14315, #12584, .T. ) ;
#20841 = ADVANCED_FACE ( 'NONE', ( #6512 ), #16473, .T. ) ;
#20842 = DIRECTION ( 'NONE',  ( 0.000000000000000000, 0.000000000000000000, -1.000000000000000000 ) ) ;
#20843 = CARTESIAN_POINT ( 'NONE',  ( -1.878215178124998497, 27.69062499938548427, 12.25316411605951927 ) ) ;
#20844 = CARTESIAN_POINT ( 'NONE',  ( 20.82877788845545552, 18.17258051049600454, 5.746835883940462963 ) ) ;
#20845 = CARTESIAN_POINT ( 'NONE',  ( 4.000000000000003553, 26.78124999877097068, 6.690598923241489970 ) ) ;
#20846 = AXIS2_PLACEMENT_3D ( 'NONE', #3215, #2973, #8719 ) ;
#20847 = ORIENTED_EDGE ( 'NONE', *, *, #24592, .F. ) ;
#20848 = CARTESIAN_POINT ( 'NONE',  ( 0.000000000000000000, 6.000000000000000000, 20.00000000000000000 ) ) ;
#20849 = CARTESIAN_POINT ( 'NONE',  ( -3.999999999999995559, 29.23750000000000071, 6.690598923241487306 ) ) ;
#20850 = CARTESIAN_POINT ( 'NONE',  ( -3.756430356250003655, -26.49062499938548498, 8.999999999999992895 ) ) ;
#20851 = FACE_OUTER_BOUND ( 'NONE', #1207, .T. ) ;
#20852 = CARTESIAN_POINT ( 'NONE',  ( 3.756430356250003655, 26.60312499938548569, 8.999999999999992895 ) ) ;
#20853 = CARTESIAN_POINT ( 'NONE',  ( 3.959305739469038251E-15, 30.00000000000000355, 12.99999999999999289 ) ) ;
#20855 = ORIENTED_EDGE ( 'NONE', *, *, #23843, .T. ) ;
#20854 = CARTESIAN_POINT ( 'NONE',  ( 1.878215178125000939, -12.25316411605952283, 0.5156249993854833402 ) ) ;
#20856 = ORIENTED_EDGE ( 'NONE', *, *, #5845, .T. ) ;
#20857 = CARTESIAN_POINT ( 'NONE',  ( 0.000000000000000000, 0.000000000000000000, -6.500000000000000000 ) ) ;
#20858 = CARTESIAN_POINT ( 'NONE',  ( 2.000000000000003553, 27.32500000000000995, 5.535898384862238508 ) ) ;
#20859 = CIRCLE ( 'NONE', #25445, 0.5000000000000005551 ) ;
#20860 = ORIENTED_EDGE ( 'NONE', *, *, #21994, .F. ) ;
#20861 = CARTESIAN_POINT ( 'NONE',  ( 3.834746474454188013E-15, 25.56250000000000000, 4.999999999999992006 ) ) ;
#20862 = CARTESIAN_POINT ( 'NONE',  ( 19.98460540328483859, 19.98460540328476398, 4.999999999999992006 ) ) ;
#20863 = CARTESIAN_POINT ( 'NONE',  ( 0.000000000000000000, 0.000000000000000000, -6.500000000000000000 ) ) ;
#20864 = CIRCLE ( 'NONE', #3739, 0.4999999999999999445 ) ;
#20865 = AXIS2_PLACEMENT_3D ( 'NONE', #10044, #8101, #24042 ) ;
#20866 = DIRECTION ( 'NONE',  ( -0.000000000000000000, -0.000000000000000000, 1.000000000000000000 ) ) ;
#20867 = CARTESIAN_POINT ( 'NONE',  ( 1.878215178124998275, 28.21562499938549351, 12.25316411605952283 ) ) ;
#20868 = ADVANCED_FACE ( 'NONE', ( #4061 ), #641, .F. ) ;
#20870 = EDGE_CURVE ( 'NONE', #10843, #8456, #517, .T. ) ;
#20869 = AXIS2_PLACEMENT_3D ( 'NONE', #11087, #1286, #1149 ) ;
#20871 = AXIS2_PLACEMENT_3D ( 'NONE', #14581, #18518, #18759 ) ;
#20872 = DIRECTION ( 'NONE',  ( 0.000000000000000000, 0.000000000000000000, 1.000000000000000000 ) ) ;
#20873 = DIRECTION ( 'NONE',  ( 0.000000000000000000, 0.000000000000000000, 1.000000000000000000 ) ) ;
#20874 = CYLINDRICAL_SURFACE ( 'NONE', #18775, 0.5000000000000004441 ) ;
#20875 = EDGE_CURVE ( 'NONE', #3398, #2759, #18334, .T. ) ;
#20876 = CARTESIAN_POINT ( 'NONE',  ( 4.000000000000003553, -8.999999999999992895, 3.093749998770968457 ) ) ;
#20877 = CARTESIAN_POINT ( 'NONE',  ( 3.756430356250003211, 25.62812499938548072, 6.831223922626973533 ) ) ;
#20878 = AXIS2_PLACEMENT_3D ( 'NONE', #19849, #25489, #19733 ) ;
#20879 = CARTESIAN_POINT ( 'NONE',  ( 1.071796769724481901, -28.41115380933862866, 12.99999999999999645 ) ) ;
#20880 = CARTESIAN_POINT ( 'NONE',  ( 21.38562447863985483, 18.72942710068040739, 5.746835883940462963 ) ) ;
#20881 = CARTESIAN_POINT ( 'NONE',  ( 21.75912901301770219, 16.44673425709888548, 11.16877607737301226 ) ) ;
#20882 = CARTESIAN_POINT ( 'NONE',  ( -21.28941499438242246, -22.67092431280570963, 1.000000000000000000 ) ) ;
#20883 = DIRECTION ( 'NONE',  ( 0.000000000000000000, 1.000000000000000000, 0.000000000000000000 ) ) ;
#20884 = CARTESIAN_POINT ( 'NONE',  ( 1.878215178125004048, 28.81562499938548427, 5.746835883940462963 ) ) ;
#20885 = CIRCLE ( 'NONE', #13372, 0.4999999999999993339 ) ;
#20886 = DIRECTION ( 'NONE',  ( 1.000000000000000000, 0.000000000000000000, 0.000000000000000000 ) ) ;
#20887 = CARTESIAN_POINT ( 'NONE',  ( 20.74922837557196331, 18.09303099761251588, 5.746835883940462963 ) ) ;
#20888 = DIRECTION ( 'NONE',  ( -1.000000000000000000, -0.000000000000000000, -0.000000000000000000 ) ) ;
#20889 = ORIENTED_EDGE ( 'NONE', *, *, #17323, .F. ) ;
#20890 = LINE ( 'NONE', #22601, #23040 ) ;
#20891 = CARTESIAN_POINT ( 'NONE',  ( 4.000000000000003553, 27.64374999877096784, 8.999999999999992895 ) ) ;
#20892 = CARTESIAN_POINT ( 'NONE',  ( 3.756430356249996994, -28.06562499938548427, 8.999999999999992895 ) ) ;
#20894 = ORIENTED_EDGE ( 'NONE', *, *, #16662, .T. ) ;
#20893 = CARTESIAN_POINT ( 'NONE',  ( 3.369928719974892281E-15, 25.50624999877096855, 4.999999999999992006 ) ) ;
#20895 = CARTESIAN_POINT ( 'NONE',  ( -27.10000000000000497, -0.5999999999999998668, 19.59999999999999787 ) ) ;
#20896 = VECTOR ( 'NONE', #2132, 1000.000000000000000 ) ;
#20897 = ORIENTED_EDGE ( 'NONE', *, *, #3811, .F. ) ;
#20898 = CARTESIAN_POINT ( 'NONE',  ( -1.878215178125000939, -29.11562499938548498, 12.25316411605952283 ) ) ;
#20899 = VERTEX_POINT ( 'NONE', #22860 ) ;
#20900 = ORIENTED_EDGE ( 'NONE', *, *, #21998, .T. ) ;
#20901 = DIRECTION ( 'NONE',  ( 1.000000000000000000, 0.000000000000000000, 0.000000000000000000 ) ) ;
#20902 = CARTESIAN_POINT ( 'NONE',  ( -3.756430356249994329, 28.59062499938548996, 6.831223922626973533 ) ) ;
#20903 = AXIS2_PLACEMENT_3D ( 'NONE', #15916, #25718, #15778 ) ;
#20904 = DIRECTION ( 'NONE',  ( 0.000000000000000000, -0.000000000000000000, 1.000000000000000000 ) ) ;
#20905 = EDGE_CURVE ( 'NONE', #1309, #23985, #4935, .T. ) ;
#20906 = EDGE_CURVE ( 'NONE', #15602, #5488, #6777, .T. ) ;
#20907 = CIRCLE ( 'NONE', #12978, 31.10000000000000142 ) ;
#20908 = CARTESIAN_POINT ( 'NONE',  ( 1.878215178125000939, -12.25316411605952283, 2.428124999385484539 ) ) ;
#20909 = PRESENTATION_STYLE_ASSIGNMENT (( #12930 ) ) ;
#20910 = CARTESIAN_POINT ( 'NONE',  ( 0.000000000000000000, 0.000000000000000000, 1.000000000000000000 ) ) ;
#20911 = CARTESIAN_POINT ( 'NONE',  ( 1.878215178125000939, 29.11562499938548498, 12.25316411605952283 ) ) ;
#20912 = CIRCLE ( 'NONE', #16763, 0.5000000000000002220 ) ;
#20913 = CARTESIAN_POINT ( 'NONE',  ( 23.39639562250992810, 17.73954137301747380, 6.690598923241489970 ) ) ;
#20914 = CARTESIAN_POINT ( 'NONE',  ( 0.000000000000000000, 0.000000000000000000, 1.000000000000000000 ) ) ;
#20915 = UNCERTAINTY_MEASURE_WITH_UNIT (LENGTH_MEASURE( 1.000000000000000082E-05 ), #19068, 'distance_accuracy_value', 'NONE');
#20916 = PRODUCT_DEFINITION_CONTEXT ( 'detailed design', #12618, 'design' ) ;
#20917 = CARTESIAN_POINT ( 'NONE',  ( 3.756430356250003655, 27.84062499938548640, 8.999999999999992895 ) ) ;
#20918 = SURFACE_STYLE_USAGE ( .BOTH. , #9015 ) ;
#20919 = CARTESIAN_POINT ( 'NONE',  ( -23.96296185032681336, 19.82388608118453632, -6.500000000000000000 ) ) ;
#20920 = CARTESIAN_POINT ( 'NONE',  ( 21.21320343559646915, 21.21320343559638744, 4.999999999999992006 ) ) ;
#20921 = FACE_OUTER_BOUND ( 'NONE', #14628, .T. ) ;
#20922 = CARTESIAN_POINT ( 'NONE',  ( -3.756430356250004099, -27.09062499938548285, 6.831223922626973533 ) ) ;
#20923 =( BOUNDED_CURVE ( )  B_SPLINE_CURVE ( 2, ( #25416, #5553, #9595, #13537, #17582, #15628, #22013, #2277, #6184 ),
 .UNSPECIFIED., .F., .F. ) 
 B_SPLINE_CURVE_WITH_KNOTS ( ( 3, 2, 2, 2, 3 ),
 ( 0.4250000000000000444, 0.4333333333333333481, 0.4500000000000000111, 0.4666666666666666741, 0.4750000000000000333 ),
 .UNSPECIFIED. ) 
 CURVE ( )  GEOMETRIC_REPRESENTATION_ITEM ( )  RATIONAL_B_SPLINE_CURVE ( ( 0.9330127018922194093, 0.9330127018922196314, 1.000000000000000000, 0.8660254037844387076, 1.000000000000000000, 0.8660254037844387076, 1.000000000000000000, 0.9330127018922191873, 0.9330127018922194093 ) ) 
 REPRESENTATION_ITEM ( '' )  );
#20924 = CARTESIAN_POINT ( 'NONE',  ( 3.735045420075836212E-15, 25.36562499938548498, 4.662447845253954171 ) ) ;
#20926 = EDGE_CURVE ( 'NONE', #19323, #9003, #8877, .T. ) ;
#20925 = DIRECTION ( 'NONE',  ( 0.000000000000000000, 0.000000000000000000, 1.000000000000000000 ) ) ;
#20927 = AXIS2_PLACEMENT_3D ( 'NONE', #956, #11130, #25137 ) ;
#20928 = LINE ( 'NONE', #18965, #2894 ) ;
#20929 = CARTESIAN_POINT ( 'NONE',  ( -7.234255490827218082, -30.12293631110037140, -6.500000000000000000 ) ) ;
#20930 = VERTEX_POINT ( 'NONE', #18941 ) ;
#20931 = CARTESIAN_POINT ( 'NONE',  ( 21.21320343559646915, 21.21320343559638744, 4.999999999999992006 ) ) ;
#20933 = VERTEX_POINT ( 'NONE', #8999 ) ;
#20932 = FACE_OUTER_BOUND ( 'NONE', #13985, .T. ) ;
#20934 = AXIS2_PLACEMENT_3D ( 'NONE', #10035, #6114, #8212 ) ;
#20935 = CIRCLE ( 'NONE', #6713, 26.00000000000000355 ) ;
#20936 = ORIENTED_EDGE ( 'NONE', *, *, #3860, .T. ) ;
#20937 = ORIENTED_EDGE ( 'NONE', *, *, #11521, .T. ) ;
#20938 = ORIENTED_EDGE ( 'NONE', *, *, #10581, .F. ) ;
#20939 = VERTEX_POINT ( 'NONE', #24434 ) ;
#20940 = CARTESIAN_POINT ( 'NONE',  ( 31.06601413805602618, 1.453535542772499856, -2.750000000000000000 ) ) ;
#20941 = CIRCLE ( 'NONE', #15098, 31.10000000000000142 ) ;
#20942 = ORIENTED_EDGE ( 'NONE', *, *, #1314, .F. ) ;
#20943 = LINE ( 'NONE', #10855, #7750 ) ;
#20944 = CARTESIAN_POINT ( 'NONE',  ( 3.756430356250002323, 29.26562499938548356, 11.16877607737301403 ) ) ;
#20945 = VECTOR ( 'NONE', #4628, 1000.000000000000000 ) ;
#20946 = CARTESIAN_POINT ( 'NONE',  ( 3.756430356250003655, -8.999999999999992895, 4.303124999385482319 ) ) ;
#20947 = CARTESIAN_POINT ( 'NONE',  ( -1.999999999999995781, -5.535898384862237620, 0.5437499987709683014 ) ) ;
#20948 = PRODUCT_DEFINITION_SHAPE ( 'NONE', 'NONE',  #25886 ) ;
#20949 = CARTESIAN_POINT ( 'NONE',  ( 17.85210898470722896, 23.16450374062589646, 11.16877607737301226 ) ) ;
#20950 = AXIS2_PLACEMENT_3D ( 'NONE', #21028, #24686, #20760 ) ;
#20951 = FACE_OUTER_BOUND ( 'NONE', #3777, .T. ) ;
#20952 = VECTOR ( 'NONE', #15548, 1000.000000000000000 ) ;
#20953 = CARTESIAN_POINT ( 'NONE',  ( 20.67279826512042362, -15.85973458909328571, 20.00001200000000523 ) ) ;
#20955 = ADVANCED_FACE ( 'NONE', ( #24691 ), #2114, .T. ) ;
#20954 = CARTESIAN_POINT ( 'NONE',  ( 2.672651547586948120E-15, -13.33755215474602984, 3.178124999385481431 ) ) ;
#20956 = DIRECTION ( 'NONE',  ( -0.5358267949789882190, 0.8443279255020205154, 0.000000000000000000 ) ) ;
#20957 = CARTESIAN_POINT ( 'NONE',  ( 4.000000000000003553, -8.999999999999992895, 4.049999999999998046 ) ) ;
#20958 = DIRECTION ( 'NONE',  ( 0.06279051952932236669, 0.9980267284282710039, 0.000000000000000000 ) ) ;
#20959 = LINE ( 'NONE', #16638, #25539 ) ;
#20960 = CARTESIAN_POINT ( 'NONE',  ( 1.878215178125000939, -12.25316411605952283, 3.328124999385485783 ) ) ;
#20961 = DIRECTION ( 'NONE',  ( 0.000000000000000000, 0.000000000000000000, 1.000000000000000000 ) ) ;
#20962 = CARTESIAN_POINT ( 'NONE',  ( 3.752267015613588906E-15, -4.381197846482986158, 4.106249998770967302 ) ) ;
#20963 = VERTEX_POINT ( 'NONE', #3495 ) ;
#20964 = ORIENTED_EDGE ( 'NONE', *, *, #2578, .F. ) ;
#20965 = EDGE_CURVE ( 'NONE', #10854, #21434, #3112, .T. ) ;
#20966 = AXIS2_PLACEMENT_3D ( 'NONE', #21740, #20022, #19778 ) ;
#20967 = ORIENTED_EDGE ( 'NONE', *, *, #22768, .T. ) ;
#20968 = DIRECTION ( 'NONE',  ( 0.000000000000000000, 1.000000000000000000, 0.000000000000000000 ) ) ;
#20969 = EDGE_LOOP ( 'NONE', ( #24589, #1227, #21919, #286 ) ) ;
#20970 = CARTESIAN_POINT ( 'NONE',  ( -1.878215178125000939, -26.07812499938548356, 12.25316411605952283 ) ) ;
#20971 = VERTEX_POINT ( 'NONE', #15154 ) ;
#20972 = CARTESIAN_POINT ( 'NONE',  ( 0.000000000000000000, 10.00000000000000000, 13.00000000000000178 ) ) ;
#20973 = CIRCLE ( 'NONE', #4245, 31.10000000000000142 ) ;
#20974 = VECTOR ( 'NONE', #9746, 1000.000000000000000 ) ;
#20975 = VERTEX_POINT ( 'NONE', #15010 ) ;
#20976 = CARTESIAN_POINT ( 'NONE',  ( 1.071796769724488563, -29.36740381056767291, 12.99999999999999289 ) ) ;
#20977 = CARTESIAN_POINT ( 'NONE',  ( -1.999999999999995781, 25.60000000000000142, 5.535898384862237620 ) ) ;
#20978 = CARTESIAN_POINT ( 'NONE',  ( 1.859271017917182139E-15, 27.08124999877096784, 12.99999999999999289 ) ) ;
#20979 = AXIS2_PLACEMENT_3D ( 'NONE', #13079, #19077, #16882 ) ;
#20980 = CARTESIAN_POINT ( 'NONE',  ( 2.000000000000003997, 26.42500000000000071, 5.535898384862238508 ) ) ;
#20981 = CARTESIAN_POINT ( 'NONE',  ( 15.96293558528635081, 21.61978983477866478, 8.999999999999992895 ) ) ;
#20982 = CARTESIAN_POINT ( 'NONE',  ( 19.04989862646933929, 19.04989862646927534, 13.33755215474602984 ) ) ;
#20983 = B_SPLINE_CURVE_WITH_KNOTS ( 'NONE', 3,
 ( #2422, #4386, #12367, #6481, #8454, #10142 ),
 .UNSPECIFIED., .F., .F.,
 ( 4, 2, 4 ),
 ( 0.001259672601285470291, 0.001557997829463299462, 0.001856323057641128850 ),
 .UNSPECIFIED. ) ;
#20984 = CARTESIAN_POINT ( 'NONE',  ( 9.133673601486471227, 29.72853858738282185, -2.750000000000000000 ) ) ;
#20985 = VECTOR ( 'NONE', #16507, 1000.000000000000000 ) ;
#20986 = CARTESIAN_POINT ( 'NONE',  ( -3.999999999999997335, 26.16250000000000142, 11.30940107675849404 ) ) ;
#20987 = VECTOR ( 'NONE', #25854, 1000.000000000000000 ) ;
#20988 = EDGE_CURVE ( 'NONE', #18357, #20366, #19568, .T. ) ;
#20989 = CARTESIAN_POINT ( 'NONE',  ( 18.73170057493538820, 18.73170057493532425, 13.33755215474603162 ) ) ;
#20990 = CYLINDRICAL_SURFACE ( 'NONE', #18702, 4.000000000000000000 ) ;
#20991 = ORIENTED_EDGE ( 'NONE', *, *, #5772, .T. ) ;
#20992 = EDGE_CURVE ( 'NONE', #5942, #4929, #24952, .T. ) ;
#20993 = CARTESIAN_POINT ( 'NONE',  ( 4.000000000000005329, 28.05624999877097281, 11.30940107675849760 ) ) ;
#20994 = CARTESIAN_POINT ( 'NONE',  ( 3.756430356249996105, -27.12812499938548427, 6.831223922626973533 ) ) ;
#20995 = DIRECTION ( 'NONE',  ( -0.000000000000000000, -0.000000000000000000, 1.000000000000000000 ) ) ;
#20996 = CARTESIAN_POINT ( 'NONE',  ( -3.756430356249996994, 28.17812499938548498, 8.999999999999992895 ) ) ;
#20997 = LINE ( 'NONE', #24786, #23402 ) ;
#20998 = ADVANCED_FACE ( 'NONE', ( #12365 ), #2691, .T. ) ;
#21000 = ORIENTED_EDGE ( 'NONE', *, *, #8327, .T. ) ;
#20999 = CARTESIAN_POINT ( 'NONE',  ( 1.878215178125008489, 28.92812499938549209, 5.746835883940462963 ) ) ;
#21001 = ORIENTED_EDGE ( 'NONE', *, *, #2302, .T. ) ;
#21002 = DIRECTION ( 'NONE',  ( 0.000000000000000000, 0.000000000000000000, 1.000000000000000000 ) ) ;
#21003 = PRESENTATION_LAYER_ASSIGNMENT (  '', '', ( #18080 ) ) ;
#21004 = CARTESIAN_POINT ( 'NONE',  ( 5.112995299272250684E-15, 27.36250000000000426, 4.999999999999992006 ) ) ;
#21005 = VERTEX_POINT ( 'NONE', #10651 ) ;
#21006 = CARTESIAN_POINT ( 'NONE',  ( -1.999999999999995781, 25.60000000000000142, 5.535898384862237620 ) ) ;
#21007 = CARTESIAN_POINT ( 'NONE',  ( 2.000000000000000888, 25.82499999999999929, 12.46410161513774817 ) ) ;
#21008 = CARTESIAN_POINT ( 'NONE',  ( 4.006172263299091013E-15, 25.70312499938548356, 4.662447845253954171 ) ) ;
#21009 = AXIS2_PLACEMENT_3D ( 'NONE', #8939, #20065, #16155 ) ;
#21010 = CARTESIAN_POINT ( 'NONE',  ( 27.00874656207294322, -15.41874213889423828, -6.500000000000000000 ) ) ;
#21011 = CARTESIAN_POINT ( 'NONE',  ( 4.006172263299091013E-15, 25.56250000000000711, 4.381197846482986158 ) ) ;
#21012 = AXIS2_PLACEMENT_3D ( 'NONE', #18624, #8677, #16803 ) ;
#21013 = CARTESIAN_POINT ( 'NONE',  ( 3.469446951953614189E-15, 38.49999999999999289, 8.999999999999992895 ) ) ;
#21014 = PRODUCT_CONTEXT ( 'NONE', #3250, 'mechanical' ) ;
#21015 = CYLINDRICAL_SURFACE ( 'NONE', #2069, 4.000000000000000000 ) ;
#21016 = DIRECTION ( 'NONE',  ( 1.000000000000000000, 0.000000000000000000, 0.000000000000000000 ) ) ;
#21017 = AXIS2_PLACEMENT_3D ( 'NONE', #14832, #8808, #3176 ) ;
#21018 = CARTESIAN_POINT ( 'NONE',  ( 1.878215178125004048, 25.66562499938548569, 5.746835883940462963 ) ) ;
#21019 = CARTESIAN_POINT ( 'NONE',  ( 18.99023649137219039, 18.99023649137212999, 4.999999999999991118 ) ) ;
#21020 = CARTESIAN_POINT ( 'NONE',  ( 21.70382253017380592, 19.04762515221435493, 5.746835883940462963 ) ) ;
#21021 = CARTESIAN_POINT ( 'NONE',  ( 17.27101936448323016, 19.92721674244253549, 5.746835883940462963 ) ) ;
#21022 = DIRECTION ( 'NONE',  ( 0.000000000000000000, 0.000000000000000000, 1.000000000000000000 ) ) ;
#21023 = CARTESIAN_POINT ( 'NONE',  ( -3.756430356249995661, 26.67812499938548498, 6.831223922626973533 ) ) ;
#21024 = DIRECTION ( 'NONE',  ( 1.000000000000000000, 0.000000000000000000, 0.000000000000000000 ) ) ;
#21025 = CARTESIAN_POINT ( 'NONE',  ( 22.66069015903055117, 17.34829540311172735, 8.999999999999992895 ) ) ;
#21026 = LINE ( 'NONE', #10943, #6291 ) ;
#21027 = VERTEX_POINT ( 'NONE', #16824 ) ;
#21028 = CARTESIAN_POINT ( 'NONE',  ( 0.000000000000000000, 0.000000000000000000, 30.00000000000000355 ) ) ;
#21029 = CARTESIAN_POINT ( 'NONE',  ( 2.620986760973688460E-15, 28.43124999877096926, 13.61880215351699874 ) ) ;
#21030 = CARTESIAN_POINT ( 'NONE',  ( -3.756430356250004099, -27.87812499938548427, 6.831223922626973533 ) ) ;
#21031 = EDGE_CURVE ( 'NONE', #18048, #9980, #14729, .T. ) ;
#21033 = ORIENTED_EDGE ( 'NONE', *, *, #9213, .F. ) ;
#21032 = LINE ( 'NONE', #5203, #9184 ) ;
#21034 = DIRECTION ( 'NONE',  ( 1.000000000000000000, 0.000000000000000000, 0.000000000000000000 ) ) ;
#21035 = EDGE_CURVE ( 'NONE', #1277, #23707, #4787, .T. ) ;
#21036 = AXIS2_PLACEMENT_3D ( 'NONE', #13353, #15703, #13223 ) ;
#21037 = EDGE_LOOP ( 'NONE', ( #8383, #5356, #18004, #24460 ) ) ;
#21038 = CARTESIAN_POINT ( 'NONE',  ( -3.756430356250004099, -29.22812499938548925, 6.831223922626973533 ) ) ;
#21039 = ORIENTED_EDGE ( 'NONE', *, *, #6317, .F. ) ;
#21040 = VERTEX_POINT ( 'NONE', #2559 ) ;
#21041 = CARTESIAN_POINT ( 'NONE',  ( 21.21320343559646915, 21.21320343559638744, 4.999999999999992006 ) ) ;
#21042 = EDGE_CURVE ( 'NONE', #8072, #6479, #24804, .T. ) ;
#21043 = CARTESIAN_POINT ( 'NONE',  ( -1.878215178124994722, 26.75312499938549138, 5.746835883940462963 ) ) ;
#21044 = VECTOR ( 'NONE', #4554, 1000.000000000000000 ) ;
#21045 = CARTESIAN_POINT ( 'NONE',  ( 1.878215178125000939, -12.25316411605952283, 0.5156249993854833402 ) ) ;
#21046 = CARTESIAN_POINT ( 'NONE',  ( -1.878215178124998497, -12.25316411605951927, 4.603124999385483918 ) ) ;
#21047 = DIRECTION ( 'NONE',  ( 0.000000000000000000, 0.000000000000000000, 1.000000000000000000 ) ) ;
#21048 = CARTESIAN_POINT ( 'NONE',  ( 2.672651547586948120E-15, 29.07812499938548001, 13.33755215474602984 ) ) ;
#21049 = CARTESIAN_POINT ( 'NONE',  ( 1.071796769724490783, 28.95759618943234059, 12.99999999999999467 ) ) ;
#21050 = CARTESIAN_POINT ( 'NONE',  ( 3.469446951953614189E-15, -8.999999999999992895, -10.00000000000000000 ) ) ;
#21051 = CARTESIAN_POINT ( 'NONE',  ( 1.878215178125004048, 28.36562499938548143, 5.746835883940462963 ) ) ;
#21052 = CARTESIAN_POINT ( 'NONE',  ( 3.878215178125005380, 29.57031249969274356, 8.999999999999992895 ) ) ;
#21053 = CARTESIAN_POINT ( 'NONE',  ( -1.999999999999998224, -12.46410161513774639, 0.6937499987709692117 ) ) ;
#21054 = CARTESIAN_POINT ( 'NONE',  ( 0.000000000000000000, 0.000000000000000000, -6.500000000000000000 ) ) ;
#21055 = CARTESIAN_POINT ( 'NONE',  ( -2.672651547586948120E-15, -27.39062499938548356, 13.33755215474602984 ) ) ;
#21056 = CARTESIAN_POINT ( 'NONE',  ( -3.756430356249996994, 26.37812499938548783, 8.999999999999992895 ) ) ;
#21057 = FACE_OUTER_BOUND ( 'NONE', #15302, .T. ) ;
#21058 = CARTESIAN_POINT ( 'NONE',  ( -17.78012134629613783, -25.16042852506070560, -6.500000000000000000 ) ) ;
#21059 = EDGE_CURVE ( 'NONE', #23121, #56, #8739, .T. ) ;
#21060 = DIRECTION ( 'NONE',  ( 0.000000000000000000, -0.000000000000000000, 1.000000000000000000 ) ) ;
#21061 = ORIENTED_EDGE ( 'NONE', *, *, #9720, .F. ) ;
#21062 = PLANE ( 'NONE',  #23788 ) ;
#21064 = ORIENTED_EDGE ( 'NONE', *, *, #21233, .F. ) ;
#21063 = CARTESIAN_POINT ( 'NONE',  ( -4.648177544792955347E-16, 26.85624999877096997, 4.999999999999991118 ) ) ;
#21065 = EDGE_CURVE ( 'NONE', #24237, #15562, #8837, .T. ) ;
#21066 = ORIENTED_EDGE ( 'NONE', *, *, #15240, .F. ) ;
#21067 = ORIENTED_EDGE ( 'NONE', *, *, #24600, .F. ) ;
#21068 = ORIENTED_EDGE ( 'NONE', *, *, #431, .T. ) ;
#21069 = VERTEX_POINT ( 'NONE', #18256 ) ;
#21070 = CARTESIAN_POINT ( 'NONE',  ( 0.000000000000000000, 0.000000000000000000, -6.500000000000000000 ) ) ;
#21071 = DIRECTION ( 'NONE',  ( 0.000000000000000000, 0.000000000000000000, 1.000000000000000000 ) ) ;
#21072 = PRODUCT_DEFINITION_FORMATION_WITH_SPECIFIED_SOURCE ( 'ANY', '', #7967, .NOT_KNOWN. ) ;
#21073 = CARTESIAN_POINT ( 'NONE',  ( 2.672651547586948120E-15, 28.29062499938548925, 13.33755215474603162 ) ) ;
#21074 = EDGE_CURVE ( 'NONE', #14690, #21434, #19448, .T. ) ;
#21075 = CARTESIAN_POINT ( 'NONE',  ( 1.878215178125000939, -12.25316411605952283, 4.228124999385483918 ) ) ;
#21076 = CARTESIAN_POINT ( 'NONE',  ( -3.999999999999997335, -11.30940107675849404, 2.006249998770964993 ) ) ;
#21077 = CARTESIAN_POINT ( 'NONE',  ( 0.000000000000000000, 0.000000000000000000, 18.19999999999999929 ) ) ;
#21078 = CARTESIAN_POINT ( 'NONE',  ( 3.756430356250002323, 27.01562499938548356, 11.16877607737301226 ) ) ;
#21079 = CARTESIAN_POINT ( 'NONE',  ( -17.18149551509900519, -19.58805710660146104, 20.00001200000000523 ) ) ;
#21080 = CARTESIAN_POINT ( 'NONE',  ( 1.878215178125000939, -12.25316411605952283, 4.565624999385481608 ) ) ;
#21081 = FACE_OUTER_BOUND ( 'NONE', #6240, .T. ) ;
#21082 = CARTESIAN_POINT ( 'NONE',  ( -24.86329371854747805, 18.68225429291759099, -2.750000000000000000 ) ) ;
#21083 = CARTESIAN_POINT ( 'NONE',  ( -31.03863125411922752, 1.952785157361987878, -6.500000000000000000 ) ) ;
#21084 = FACE_OUTER_BOUND ( 'NONE', #23743, .T. ) ;
#21085 = CARTESIAN_POINT ( 'NONE',  ( 3.756430356250002323, -11.16877607737301403, 4.715624999385485516 ) ) ;
#21086 = CARTESIAN_POINT ( 'NONE',  ( 23.82728881686095335, 18.17043456736849549, 8.999999999999992895 ) ) ;
#21087 = CARTESIAN_POINT ( 'NONE',  ( -1.999999999999995781, -5.535898384862237620, 4.143749998770966947 ) ) ;
#21088 = EDGE_LOOP ( 'NONE', ( #11526, #19248 ) ) ;
#21089 = ORIENTED_EDGE ( 'NONE', *, *, #13478, .F. ) ;
#21090 = ORIENTED_EDGE ( 'NONE', *, *, #20870, .T. ) ;
#21091 = DIRECTION ( 'NONE',  ( 0.000000000000000000, 0.000000000000000000, 1.000000000000000000 ) ) ;
#21092 = ORIENTED_EDGE ( 'NONE', *, *, #5496, .F. ) ;
#21093 = CARTESIAN_POINT ( 'NONE',  ( -3.756430356250003655, -26.15312499938548640, 8.999999999999992895 ) ) ;
#21094 = ORIENTED_EDGE ( 'NONE', *, *, #5804, .T. ) ;
#21095 = DIRECTION ( 'NONE',  ( 1.000000000000000000, 0.000000000000000000, 0.000000000000000000 ) ) ;
#21096 = EDGE_CURVE ( 'NONE', #7582, #14460, #387, .T. ) ;
#21097 = ORIENTED_EDGE ( 'NONE', *, *, #18233, .T. ) ;
#21098 = CARTESIAN_POINT ( 'NONE',  ( 29.09636799667075024, -10.98232076577232519, 1.000000000000000000 ) ) ;
#21099 = CARTESIAN_POINT ( 'NONE',  ( -3.999999999999997335, 25.71250000000000213, 11.30940107675849404 ) ) ;
#21100 = CARTESIAN_POINT ( 'NONE',  ( -1.999999999999995781, 28.24374999877096570, 5.535898384862237620 ) ) ;
#21101 = CARTESIAN_POINT ( 'NONE',  ( 3.469446951953614189E-15, 30.00000000000000355, 4.999999999999992006 ) ) ;
#21102 = DIRECTION ( 'NONE',  ( 1.000000000000000000, 0.000000000000000000, 0.000000000000000000 ) ) ;
#21103 = CARTESIAN_POINT ( 'NONE',  ( 20.08631576820957321, 17.43011839025013288, 12.25316411605952283 ) ) ;
#21104 = DIRECTION ( 'NONE',  ( -1.000000000000000000, 0.000000000000000000, 0.000000000000000000 ) ) ;
#21105 = CARTESIAN_POINT ( 'NONE',  ( 2.000000000000003997, 26.42500000000000071, 5.535898384862238508 ) ) ;
#21106 = CARTESIAN_POINT ( 'NONE',  ( 22.13036007314063625, 16.81796531722181598, 6.831223922626973533 ) ) ;
#21107 = DIRECTION ( 'NONE',  ( -0.000000000000000000, -0.000000000000000000, -1.000000000000000000 ) ) ;
#21108 = ORIENTED_EDGE ( 'NONE', *, *, #6740, .T. ) ;
#21109 = ORIENTED_EDGE ( 'NONE', *, *, #11951, .T. ) ;
#21110 = CARTESIAN_POINT ( 'NONE',  ( -1.999999999999998224, 28.84374999877097423, 12.46410161513774639 ) ) ;
#21111 = CARTESIAN_POINT ( 'NONE',  ( 21.21320343559646915, 21.21320343559638744, 4.999999999999992006 ) ) ;
#21112 = CARTESIAN_POINT ( 'NONE',  ( -29.41953157733101065, -10.08469938919468945, 1.000000000000000000 ) ) ;
#21113 = CARTESIAN_POINT ( 'NONE',  ( -1.878215178124995832, 27.65312499938548640, 5.746835883940462963 ) ) ;
#21114 = DIRECTION ( 'NONE',  ( 0.000000000000000000, 0.000000000000000000, -1.000000000000000000 ) ) ;
#21115 = ORIENTED_EDGE ( 'NONE', *, *, #22155, .T. ) ;
#21116 = ORIENTED_EDGE ( 'NONE', *, *, #18061, .T. ) ;
#21117 = DIRECTION ( 'NONE',  ( 0.000000000000000000, 0.000000000000000000, 1.000000000000000000 ) ) ;
#21118 = EDGE_CURVE ( 'NONE', #7323, #24696, #12070, .T. ) ;
#21119 = CARTESIAN_POINT ( 'NONE',  ( 3.834746474454188013E-15, 26.40624999877096357, 4.999999999999992006 ) ) ;
#21120 = EDGE_LOOP ( 'NONE', ( #14280, #20333, #20897 ) ) ;
#21121 = CARTESIAN_POINT ( 'NONE',  ( -1.999999999999998224, 25.75000000000000355, 12.46410161513774639 ) ) ;
#21122 = CARTESIAN_POINT ( 'NONE',  ( 0.000000000000000000, 29.52812499938548640, 13.33755215474602984 ) ) ;
#21123 = CARTESIAN_POINT ( 'NONE',  ( 5.532151103383248447, 38.49999999999999289, 11.32277940608563149 ) ) ;
#21124 = EDGE_CURVE ( 'NONE', #4507, #2220, #2306, .T. ) ;
#21125 = AXIS2_PLACEMENT_3D ( 'NONE', #7066, #15309, #9158 ) ;
#21126 = CARTESIAN_POINT ( 'NONE',  ( 0.000000000000000000, 0.000000000000000000, -6.500000000000000000 ) ) ;
#21127 = CARTESIAN_POINT ( 'NONE',  ( -1.878215178124994722, 29.34062499938548640, 5.746835883940462963 ) ) ;
#21128 = EDGE_CURVE ( 'NONE', #3228, #21953, #23756, .T. ) ;
#21129 = APPLICATION_CONTEXT ( 'automotive_design' ) ;
#21130 = DIRECTION ( 'NONE',  ( 0.000000000000000000, 0.000000000000000000, 1.000000000000000000 ) ) ;
#21131 = SHAPE_DEFINITION_REPRESENTATION ( #2342, #19829 ) ;
#21132 = EDGE_CURVE ( 'NONE', #15816, #22942, #22570, .T. ) ;
#21133 =( BOUNDED_CURVE ( )  B_SPLINE_CURVE ( 2, ( #22544, #2535, #4237, #20051, #8042, #319, #14182, #592, #2285 ),
 .UNSPECIFIED., .F., .F. ) 
 B_SPLINE_CURVE_WITH_KNOTS ( ( 3, 2, 2, 2, 3 ),
 ( 0.8750000000000000000, 0.8833333333333333037, 0.9000000000000000222, 0.9166666666666666297, 0.9250000000000000444 ),
 .UNSPECIFIED. ) 
 CURVE ( )  GEOMETRIC_REPRESENTATION_ITEM ( )  RATIONAL_B_SPLINE_CURVE ( ( 0.9330127018922194093, 0.9330127018922194093, 1.000000000000000000, 0.8660254037844387076, 1.000000000000000000, 0.8660254037844387076, 1.000000000000000000, 0.9330127018922189652, 0.9330127018922194093 ) ) 
 REPRESENTATION_ITEM ( '' )  );
#21134 = CARTESIAN_POINT ( 'NONE',  ( -28.91604871112448549, 11.44867358849382910, 1.000000000000000000 ) ) ;
#21135 = CARTESIAN_POINT ( 'NONE',  ( 0.000000000000000000, 0.000000000000000000, -6.500000000000000000 ) ) ;
#21136 = CARTESIAN_POINT ( 'NONE',  ( -3.756430356249996994, 27.61562499938548143, 8.999999999999992895 ) ) ;
#21137 = CARTESIAN_POINT ( 'NONE',  ( -3.594806220554922049, -29.78401552627944326, 7.226316032987424975 ) ) ;
#21138 = CARTESIAN_POINT ( 'NONE',  ( 16.79378605318053985, 19.62221317792666753, 12.46410161513774639 ) ) ;
#21139 = CARTESIAN_POINT ( 'NONE',  ( 20.53936981547090568, 15.22697505955208896, 6.831223922626973533 ) ) ;
#21140 = CARTESIAN_POINT ( 'NONE',  ( 18.37725060138953737, 19.89300012924151417, 12.99999999999999289 ) ) ;
#21141 =( BOUNDED_CURVE ( )  B_SPLINE_CURVE ( 2, ( #18869, #4867, #3283, #15206, #23174, #21204, #11255, #19239, #1341 ),
 .UNSPECIFIED., .F., .F. ) 
 B_SPLINE_CURVE_WITH_KNOTS ( ( 3, 2, 2, 2, 3 ),
 ( 0.02500000000000000139, 0.03333333333333333287, 0.05000000000000000278, 0.06666666666666666574, 0.07500000000000001110 ),
 .UNSPECIFIED. ) 
 CURVE ( )  GEOMETRIC_REPRESENTATION_ITEM ( )  RATIONAL_B_SPLINE_CURVE ( ( 0.9330127018922194093, 0.9330127018922194093, 1.000000000000000000, 0.8660254037844387076, 1.000000000000000000, 0.8660254037844387076, 1.000000000000000000, 0.9330127018922191873, 0.9330127018922192983 ) ) 
 REPRESENTATION_ITEM ( '' )  );
#21142 = CARTESIAN_POINT ( 'NONE',  ( -1.878215178124995832, 27.09062499938548640, 5.746835883940462963 ) ) ;
#21143 = LINE ( 'NONE', #883, #11635 ) ;
#21144 = CARTESIAN_POINT ( 'NONE',  ( 17.82786595466764012, 20.48406333262694190, 5.746835883940462963 ) ) ;
#21145 = DIRECTION ( 'NONE',  ( 0.000000000000000000, 0.000000000000000000, 1.000000000000000000 ) ) ;
#21146 = ORIENTED_EDGE ( 'NONE', *, *, #10271, .T. ) ;
#21147 = AXIS2_PLACEMENT_3D ( 'NONE', #19812, #3993, #17602 ) ;
#21148 = CARTESIAN_POINT ( 'NONE',  ( -3.999999999999996003, 26.48124999877096641, 6.690598923241487306 ) ) ;
#21149 = CARTESIAN_POINT ( 'NONE',  ( 4.000000000000003553, 27.19374999877096855, 8.999999999999992895 ) ) ;
#21150 = CARTESIAN_POINT ( 'NONE',  ( -1.878215178125000939, -28.66562499938548569, 12.25316411605952283 ) ) ;
#21152 = ORIENTED_EDGE ( 'NONE', *, *, #197, .T. ) ;
#21151 = DIRECTION ( 'NONE',  ( 0.000000000000000000, 1.000000000000000000, -0.000000000000000000 ) ) ;
#21153 = CARTESIAN_POINT ( 'NONE',  ( 1.878215178125004048, 25.32812499938548356, 5.746835883940462963 ) ) ;
#21154 = EDGE_LOOP ( 'NONE', ( #3453, #969, #5266, #16405 ) ) ;
#21155 = CARTESIAN_POINT ( 'NONE',  ( 3.756430356249996994, -27.16562499938548214, 8.999999999999992895 ) ) ;
#21156 = ORIENTED_EDGE ( 'NONE', *, *, #6419, .F. ) ;
#21157 = ORIENTED_EDGE ( 'NONE', *, *, #2599, .T. ) ;
#21158 = LINE ( 'NONE', #9506, #18505 ) ;
#21159 = CARTESIAN_POINT ( 'NONE',  ( 0.000000000000000000, 28.29062499938548925, 13.33755215474602984 ) ) ;
#21160 = CARTESIAN_POINT ( 'NONE',  ( -3.756430356249997438, -11.16877607737301048, 1.753124999385480276 ) ) ;
#21161 = EDGE_CURVE ( 'NONE', #16896, #11078, #16299, .T. ) ;
#21162 = CARTESIAN_POINT ( 'NONE',  ( 1.071796769724487675, 29.08615380933863293, 4.999999999999988454 ) ) ;
#21163 = EDGE_CURVE ( 'NONE', #5788, #21186, #12633, .T. ) ;
#21164 = DIRECTION ( 'NONE',  ( 0.000000000000000000, 0.000000000000000000, 1.000000000000000000 ) ) ;
#21165 = EDGE_CURVE ( 'NONE', #18175, #2848, #21669, .T. ) ;
#21166 = CARTESIAN_POINT ( 'NONE',  ( 2.000000000000007105, 26.87500000000001066, 5.535898384862238508 ) ) ;
#21167 = CARTESIAN_POINT ( 'NONE',  ( -28.91604871112448549, 11.44867358849382910, -6.500000000000000000 ) ) ;
#21168 = CARTESIAN_POINT ( 'NONE',  ( 2.672651547586948120E-15, 28.17812499938548143, 13.33755215474603162 ) ) ;
#21169 = LINE ( 'NONE', #15794, #10788 ) ;
#21170 = CARTESIAN_POINT ( 'NONE',  ( 27.10000000000000142, 3.318792825689327485E-15, 0.000000000000000000 ) ) ;
#21171 = CARTESIAN_POINT ( 'NONE',  ( 5.827558883615830965, -30.54913349766226105, -6.500000000000000000 ) ) ;
#21172 = CARTESIAN_POINT ( 'NONE',  ( 3.469446951953614189E-15, 35.50000000000000711, 4.999999999999992006 ) ) ;
#21173 = CARTESIAN_POINT ( 'NONE',  ( -1.878215178125004048, -28.47812499938548569, 5.746835883940462963 ) ) ;
#21174 = CARTESIAN_POINT ( 'NONE',  ( -3.756430356249997882, 25.51562499938548356, 11.16877607737301226 ) ) ;
#21175 = CARTESIAN_POINT ( 'NONE',  ( -3.999999999999995559, 29.63124999877096855, 6.690598923241487306 ) ) ;
#21176 = LINE ( 'NONE', #3248, #20409 ) ;
#21177 = CARTESIAN_POINT ( 'NONE',  ( 0.2612076306139402004, -30.00000000000001066, 12.99999999999999467 ) ) ;
#21178 = VERTEX_POINT ( 'NONE', #1237 ) ;
#21179 = CARTESIAN_POINT ( 'NONE',  ( 2.003086131649545506E-15, 29.19062499938549138, 13.33755215474602984 ) ) ;
#21180 = DIRECTION ( 'NONE',  ( 1.000000000000000000, 0.000000000000000000, 0.000000000000000000 ) ) ;
#21182 = ORIENTED_EDGE ( 'NONE', *, *, #15926, .T. ) ;
#21181 = DIRECTION ( 'NONE',  ( 0.000000000000000000, 0.000000000000000000, 1.000000000000000000 ) ) ;
#21183 = ORIENTED_EDGE ( 'NONE', *, *, #24897, .F. ) ;
#21184 = EDGE_LOOP ( 'NONE', ( #17239, #25387, #8223, #4453, #20299, #18997, #19380, #5316, #23090 ) ) ;
#21185 = ORIENTED_EDGE ( 'NONE', *, *, #3848, .T. ) ;
#21186 = VERTEX_POINT ( 'NONE', #16948 ) ;
#21187 = DIRECTION ( 'NONE',  ( 0.000000000000000000, 0.000000000000000000, 1.000000000000000000 ) ) ;
#21188 = CARTESIAN_POINT ( 'NONE',  ( 0.000000000000000000, 0.000000000000000000, 1.000000000000000000 ) ) ;
#21189 = CARTESIAN_POINT ( 'NONE',  ( 23.65388548145850933, 18.45264921795818225, 10.59017455026297228 ) ) ;
#21190 = ADVANCED_FACE ( 'NONE', ( #25304 ), #21383, .T. ) ;
#21191 = CARTESIAN_POINT ( 'NONE',  ( 3.756430356250002323, -11.16877607737301226, 1.453124999385484228 ) ) ;
#21192 = CARTESIAN_POINT ( 'NONE',  ( -3.999999999999996003, -6.690598923241487306, 1.031249998770967347 ) ) ;
#21193 = DIRECTION ( 'NONE',  ( 0.000000000000000000, -0.000000000000000000, -1.000000000000000000 ) ) ;
#21194 = CYLINDRICAL_SURFACE ( 'NONE', #8849, 4.000000000000000000 ) ;
#21195 = ADVANCED_FACE ( 'NONE', ( #25042 ), #5422, .F. ) ;
#21196 = DIRECTION ( 'NONE',  ( -0.000000000000000000, -1.000000000000000000, -0.000000000000000000 ) ) ;
#21197 = CARTESIAN_POINT ( 'NONE',  ( 20.15576018847347584, 21.67150971632543133, 4.999999999999987566 ) ) ;
#21198 = CARTESIAN_POINT ( 'NONE',  ( -3.999999999999996003, -6.690598923241487306, 0.6374999999999966249 ) ) ;
#21199 = CARTESIAN_POINT ( 'NONE',  ( 0.000000000000000000, 0.000000000000000000, -6.500000000000000000 ) ) ;
#21200 = CARTESIAN_POINT ( 'NONE',  ( 30.63887302793247969, 5.335677986744675749, -6.500000000000000000 ) ) ;
#21201 = DIRECTION ( 'NONE',  ( -0.000000000000000000, -0.000000000000000000, 1.000000000000000000 ) ) ;
#21202 = CARTESIAN_POINT ( 'NONE',  ( 3.999999999999996003, -26.48124999877096641, 6.690598923241487306 ) ) ;
#21203 = CARTESIAN_POINT ( 'NONE',  ( 3.735045420075836212E-15, -4.662447845253954171, 4.415624999385481253 ) ) ;
#21204 = CARTESIAN_POINT ( 'NONE',  ( -3.999999999999999112, 25.26250000000000284, 11.30940107675849404 ) ) ;
#21205 = VECTOR ( 'NONE', #19334, 1000.000000000000000 ) ;
#21206 = CARTESIAN_POINT ( 'NONE',  ( 0.000000000000000000, 0.000000000000000000, 19.50000000000000000 ) ) ;
#21207 = ORIENTED_EDGE ( 'NONE', *, *, #9000, .T. ) ;
#21208 = CARTESIAN_POINT ( 'NONE',  ( 5.112995299272250684E-15, 27.36250000000000426, 4.999999999999992006 ) ) ;
#21209 = ORIENTED_EDGE ( 'NONE', *, *, #15739, .T. ) ;
#21210 = ORIENTED_EDGE ( 'NONE', *, *, #12919, .F. ) ;
#21211 = LINE ( 'NONE', #22797, #12527 ) ;
#21212 = VERTEX_POINT ( 'NONE', #3463 ) ;
#21213 = CARTESIAN_POINT ( 'NONE',  ( -3.756430356250003655, -28.40312499938548640, 8.999999999999992895 ) ) ;
#21214 = ORIENTED_EDGE ( 'NONE', *, *, #17830, .F. ) ;
#21215 = DIRECTION ( 'NONE',  ( 0.000000000000000000, 0.000000000000000000, 1.000000000000000000 ) ) ;
#21216 = ORIENTED_EDGE ( 'NONE', *, *, #23587, .T. ) ;
#21217 = CARTESIAN_POINT ( 'NONE',  ( -1.999999999999995781, 27.85000000000000142, 5.535898384862237620 ) ) ;
#21218 = CYLINDRICAL_SURFACE ( 'NONE', #9330, 0.5000000000000001110 ) ;
#21219 = DIRECTION ( 'NONE',  ( 1.000000000000000000, 0.000000000000000000, 0.000000000000000000 ) ) ;
#21220 = CYLINDRICAL_SURFACE ( 'NONE', #8756, 4.000000000000000000 ) ;
#21221 = CARTESIAN_POINT ( 'NONE',  ( 21.17576591853879719, 15.86337116261998048, 6.831223922626973533 ) ) ;
#21222 = ADVANCED_FACE ( 'NONE', ( #7130 ), #2947, .F. ) ;
#21223 = LINE ( 'NONE', #20984, #21324 ) ;
#21224 = AXIS2_PLACEMENT_3D ( 'NONE', #16359, #10833, #24452 ) ;
#21225 = CARTESIAN_POINT ( 'NONE',  ( -3.999999999999996003, 26.08750000000000213, 6.690598923241487306 ) ) ;
#21226 = EDGE_CURVE ( 'NONE', #1345, #962, #22080, .T. ) ;
#21227 = CARTESIAN_POINT ( 'NONE',  ( 16.63234978716043244, 21.94474454307910705, 8.999999999999992895 ) ) ;
#21228 = CARTESIAN_POINT ( 'NONE',  ( 1.071796769724491227, 26.83615380933863293, 4.999999999999989342 ) ) ;
#21229 = ORIENTED_EDGE ( 'NONE', *, *, #5334, .T. ) ;
#21230 = ORIENTED_EDGE ( 'NONE', *, *, #15482, .T. ) ;
#21231 = CARTESIAN_POINT ( 'NONE',  ( 4.000000000000002665, 27.60624999877096641, 11.30940107675849760 ) ) ;
#21232 = DIRECTION ( 'NONE',  ( -0.000000000000000000, -0.000000000000000000, 1.000000000000000000 ) ) ;
#21233 = EDGE_CURVE ( 'NONE', #5166, #23155, #1109, .T. ) ;
#21235 = EDGE_LOOP ( 'NONE', ( #15461, #10170, #250, #3362 ) ) ;
#21234 = CIRCLE ( 'NONE', #10354, 31.10000000000000142 ) ;
#21236 = CARTESIAN_POINT ( 'NONE',  ( -3.999999999999995559, 26.98750000000000071, 6.690598923241487306 ) ) ;
#21237 = CIRCLE ( 'NONE', #7460, 31.10000000000000142 ) ;
#21238 = CARTESIAN_POINT ( 'NONE',  ( -1.878215178124995832, 27.20312499938548711, 5.746835883940462963 ) ) ;
#21239 = CARTESIAN_POINT ( 'NONE',  ( -13.69242354489172797, -27.92360179968362743, -6.500000000000000000 ) ) ;
#21240 = ORIENTED_EDGE ( 'NONE', *, *, #19672, .T. ) ;
#21241 = ORIENTED_EDGE ( 'NONE', *, *, #6822, .F. ) ;
#21242 = FACE_OUTER_BOUND ( 'NONE', #12486, .T. ) ;
#21243 = AXIS2_PLACEMENT_3D ( 'NONE', #17553, #25528, #25390 ) ;
#21244 = CARTESIAN_POINT ( 'NONE',  ( 5.577813053751546416E-15, 25.73124999877096997, 12.99999999999999289 ) ) ;
#21245 = AXIS2_PLACEMENT_3D ( 'NONE', #1043, #15033, #9016 ) ;
#21246 = ORIENTED_EDGE ( 'NONE', *, *, #2992, .F. ) ;
#21247 = CARTESIAN_POINT ( 'NONE',  ( -3.756430356250003211, -29.34062499938548640, 6.831223922626973533 ) ) ;
#21248 = DIRECTION ( 'NONE',  ( -0.000000000000000000, 0.000000000000000000, 1.000000000000000000 ) ) ;
#21249 = CARTESIAN_POINT ( 'NONE',  ( -3.756430356249997882, 25.85312499938549635, 11.16877607737301048 ) ) ;
#21250 = CARTESIAN_POINT ( 'NONE',  ( -4.000000000000001776, -26.25624999877096855, 11.30940107675849760 ) ) ;
#21251 = CARTESIAN_POINT ( 'NONE',  ( 1.878215178125003382, 29.56562499938549138, 12.25316411605952283 ) ) ;
#21252 = VECTOR ( 'NONE', #6765, 1000.000000000000000 ) ;
#21253 = ADVANCED_BREP_SHAPE_REPRESENTATION ( '', ( #13271, #21036 ), #7676 ) ;
#21254 = CARTESIAN_POINT ( 'NONE',  ( 2.000000000000003553, 29.06874999877097210, 5.535898384862238508 ) ) ;
#21255 = VECTOR ( 'NONE', #114, 1000.000000000000000 ) ;
#21256 = APPLICATION_PROTOCOL_DEFINITION ( 'draft international standard', 'automotive_design', 1998, #3751 ) ;
#21257 = DIRECTION ( 'NONE',  ( -0.8443279255020122998, 0.5358267949790012086, 0.000000000000000000 ) ) ;
#21258 = AXIS2_PLACEMENT_3D ( 'NONE', #21902, #8293, #6073 ) ;
#21259 = FACE_OUTER_BOUND ( 'NONE', #15265, .T. ) ;
#21260 = EDGE_CURVE ( 'NONE', #13647, #6542, #14156, .T. ) ;
#21261 = CARTESIAN_POINT ( 'NONE',  ( -1.878215178124998497, 27.69062499938548427, 12.25316411605951927 ) ) ;
#21262 = CARTESIAN_POINT ( 'NONE',  ( -0.2644264925860129734, -30.00000000000001421, 4.999999999999992006 ) ) ;
#21263 = CARTESIAN_POINT ( 'NONE',  ( 20.87953742278953229, 20.87953742278945768, 13.33755215474602984 ) ) ;
#21264 = CARTESIAN_POINT ( 'NONE',  ( 17.24222938593383248, 22.55462414185250353, 6.831223922626973533 ) ) ;
#21265 = DIRECTION ( 'NONE',  ( 1.000000000000000000, 0.000000000000000000, 0.000000000000000000 ) ) ;
#21266 = CARTESIAN_POINT ( 'NONE',  ( 3.756430356250003655, 27.84062499938548640, 8.999999999999992895 ) ) ;
#21267 = CARTESIAN_POINT ( 'NONE',  ( 0.000000000000000000, 0.000000000000000000, -6.500000000000000000 ) ) ;
#21268 = CARTESIAN_POINT ( 'NONE',  ( 18.14606400620158411, 20.80226138416088588, 5.746835883940462963 ) ) ;
#21269 = CARTESIAN_POINT ( 'NONE',  ( -17.87326343783906424, 25.45105997952945387, -6.500000000000000000 ) ) ;
#21270 = EDGE_LOOP ( 'NONE', ( #13273, #16228, #15845, #22247 ) ) ;
#21271 = CARTESIAN_POINT ( 'NONE',  ( 2.000000000000003997, 25.46874999877096712, 5.535898384862238508 ) ) ;
#21272 = CARTESIAN_POINT ( 'NONE',  ( 4.000000000000001776, 29.40624999877096357, 11.30940107675849760 ) ) ;
#21273 = CARTESIAN_POINT ( 'NONE',  ( -2.672651547586948120E-15, -28.17812499938548143, 13.33755215474602984 ) ) ;
#21274 = ORIENTED_EDGE ( 'NONE', *, *, #12394, .F. ) ;
#21275 = CARTESIAN_POINT ( 'NONE',  ( -3.756430356249996105, 26.79062499938548569, 6.831223922626973533 ) ) ;
#21276 = VECTOR ( 'NONE', #6369, 1000.000000000000000 ) ;
#21277 = CIRCLE ( 'NONE', #24208, 0.5000000000000001110 ) ;
#21278 = CARTESIAN_POINT ( 'NONE',  ( -15.85973458909327860, 20.67279826512041652, 20.00001200000000168 ) ) ;
#21279 = CARTESIAN_POINT ( 'NONE',  ( -1.878215178125000939, -27.31562499938548427, 12.25316411605952283 ) ) ;
#21280 = ORIENTED_EDGE ( 'NONE', *, *, #8826, .T. ) ;
#21281 = ORIENTED_EDGE ( 'NONE', *, *, #7935, .F. ) ;
#21282 = DIRECTION ( 'NONE',  ( -0.9822872507286872779, 0.1873813145857327056, 0.000000000000000000 ) ) ;
#21283 = CARTESIAN_POINT ( 'NONE',  ( -3.756430356249994329, 26.86562499938548498, 11.16877607737301226 ) ) ;
#21284 = AXIS2_PLACEMENT_3D ( 'NONE', #13639, #9718, #5274 ) ;
#21285 = VECTOR ( 'NONE', #14722, 1000.000000000000000 ) ;
#21286 = CARTESIAN_POINT ( 'NONE',  ( 3.756430356250003655, -8.999999999999992895, 1.040624999385484584 ) ) ;
#21287 =( BOUNDED_CURVE ( )  B_SPLINE_CURVE ( 2, ( #24872, #20559, #6952, #18600, #11005, #687, #14931 ),
 .UNSPECIFIED., .F., .F. ) 
 B_SPLINE_CURVE_WITH_KNOTS ( ( 3, 2, 2, 3 ),
 ( 0.09999999999999981126, 0.1166666666666664326, 0.1333333333333330539, 0.1499999999999996891 ),
 .UNSPECIFIED. ) 
 CURVE ( )  GEOMETRIC_REPRESENTATION_ITEM ( )  RATIONAL_B_SPLINE_CURVE ( ( 1.000000000000001776, 0.8660254037844372643, 1.000000000000000000, 0.8660254037844387076, 1.000000000000000000, 0.8660254037844411501, 0.9999999999999975575 ) ) 
 REPRESENTATION_ITEM ( '' )  );
#21288 = VECTOR ( 'NONE', #23429, 1000.000000000000000 ) ;
#21289 = CARTESIAN_POINT ( 'NONE',  ( 0.000000000000000000, 0.000000000000000000, 1.000000000000000000 ) ) ;
#21290 = SURFACE_STYLE_USAGE ( .BOTH. , #13192 ) ;
#21291 = EDGE_CURVE ( 'NONE', #23177, #2690, #24916, .T. ) ;
#21292 = CARTESIAN_POINT ( 'NONE',  ( -4.000000000000003553, -27.28749999999999787, 6.690598923241489970 ) ) ;
#21293 =( BOUNDED_CURVE ( )  B_SPLINE_CURVE ( 2, ( #15372, #13422, #1119, #9095, #5187, #5305, #25433, #21396, #7518 ),
 .UNSPECIFIED., .F., .T. ) 
 B_SPLINE_CURVE_WITH_KNOTS ( ( 3, 2, 2, 2, 3 ),
 ( 0.4250000000000000444, 0.4333333333333333481, 0.4500000000000000111, 0.4666666666666666741, 0.4750000000000000333 ),
 .UNSPECIFIED. ) 
 CURVE ( )  GEOMETRIC_REPRESENTATION_ITEM ( )  RATIONAL_B_SPLINE_CURVE ( ( 0.9330127018922194093, 0.9330127018922196314, 1.000000000000000000, 0.8660254037844387076, 1.000000000000000000, 0.8660254037844387076, 1.000000000000000000, 0.9330127018922191873, 0.9330127018922194093 ) ) 
 REPRESENTATION_ITEM ( '' )  );
#21294 = AXIS2_PLACEMENT_3D ( 'NONE', #21581, #19614, #18066 ) ;
#21295 = DIRECTION ( 'NONE',  ( 0.000000000000000000, 0.000000000000000000, 1.000000000000000000 ) ) ;
#21296 = CARTESIAN_POINT ( 'NONE',  ( 25.99519186311192342, -0.5000000000000000000, 19.00000000000000000 ) ) ;
#21297 = LINE ( 'NONE', #3377, #21205 ) ;
#21298 = FACE_OUTER_BOUND ( 'NONE', #2662, .T. ) ;
#21299 = CYLINDRICAL_SURFACE ( 'NONE', #23738, 0.5000000000000004441 ) ;
#21300 = CARTESIAN_POINT ( 'NONE',  ( -4.000000000000010658, -11.30940107675848694, 0.6562499987709652371 ) ) ;
#21301 = CARTESIAN_POINT ( 'NONE',  ( -1.452785157361201396, 31.03863125411927371, 1.000000000000000000 ) ) ;
#21302 = CARTESIAN_POINT ( 'NONE',  ( -3.735045420075836212E-15, -29.41562499938548569, 4.662447845253954171 ) ) ;
#21303 = DIRECTION ( 'NONE',  ( -0.8660254037844397068, 0.000000000000000000, -0.4999999999999983347 ) ) ;
#21304 = CIRCLE ( 'NONE', #6256, 0.4999999999999998890 ) ;
#21306 = EDGE_CURVE ( 'NONE', #14582, #13859, #5800, .T. ) ;
#21305 = DIRECTION ( 'NONE',  ( 0.000000000000000000, 0.000000000000000000, 1.000000000000000000 ) ) ;
#21307 = DIRECTION ( 'NONE',  ( 0.000000000000000000, 0.000000000000000000, 1.000000000000000000 ) ) ;
#21308 = CARTESIAN_POINT ( 'NONE',  ( -30.45149776762733751, -6.317933499823126908, -2.750000000000000000 ) ) ;
#21309 = ORIENTED_EDGE ( 'NONE', *, *, #23210, .F. ) ;
#21310 = CARTESIAN_POINT ( 'NONE',  ( 3.959305671612554781E-15, 40.00000000000000000, 12.99999999999999289 ) ) ;
#21311 = DIRECTION ( 'NONE',  ( 0.000000000000000000, 0.000000000000000000, 1.000000000000000000 ) ) ;
#21313 = ORIENTED_EDGE ( 'NONE', *, *, #16545, .T. ) ;
#21312 = CARTESIAN_POINT ( 'NONE',  ( 4.648177544792954952E-15, 28.26250000000000284, 4.999999999999992006 ) ) ;
#21314 = ADVANCED_FACE ( 'NONE', ( #6993 ), #3196, .T. ) ;
#21315 = VERTEX_POINT ( 'NONE', #11164 ) ;
#21316 = VECTOR ( 'NONE', #18043, 1000.000000000000000 ) ;
#21317 = ORIENTED_EDGE ( 'NONE', *, *, #2204, .F. ) ;
#21318 = EDGE_LOOP ( 'NONE', ( #11195, #10522, #14204, #14174 ) ) ;
#21319 = ADVANCED_FACE ( 'NONE', ( #13269 ), #5038, .T. ) ;
#21320 = ORIENTED_EDGE ( 'NONE', *, *, #25301, .T. ) ;
#21321 = CARTESIAN_POINT ( 'NONE',  ( 0.000000000000000000, 0.000000000000000000, -6.500000000000000000 ) ) ;
#21322 = VECTOR ( 'NONE', #4048, 1000.000000000000000 ) ;
#21323 = CARTESIAN_POINT ( 'NONE',  ( 3.469446951953614189E-15, 40.00000000000000000, 4.999999999999992006 ) ) ;
#21324 = VECTOR ( 'NONE', #3306, 1000.000000000000000 ) ;
#21325 = CARTESIAN_POINT ( 'NONE',  ( -1.878215178124994722, 25.29062499938548925, 5.746835883940462963 ) ) ;
#21326 = CIRCLE ( 'NONE', #7953, 31.10000000000000142 ) ;
#21327 = CARTESIAN_POINT ( 'NONE',  ( 1.878215178125004048, -5.746835883940462963, 0.2156249993854816860 ) ) ;
#21328 = CARTESIAN_POINT ( 'NONE',  ( 4.000000000000001776, -11.30940107675849760, 1.256249998770964993 ) ) ;
#21329 = CARTESIAN_POINT ( 'NONE',  ( -1.071796769724494336, -25.48615380933863150, 4.999999999999992895 ) ) ;
#21330 = LINE ( 'NONE', #23283, #5860 ) ;
#21331 = CIRCLE ( 'NONE', #10047, 31.10000000000000142 ) ;
#21332 = CARTESIAN_POINT ( 'NONE',  ( 4.000000000000001776, -11.30940107675849760, 1.762499999999997957 ) ) ;
#21333 = DIRECTION ( 'NONE',  ( 1.000000000000000000, 0.000000000000000000, 0.000000000000000000 ) ) ;
#21334 = DIRECTION ( 'NONE',  ( -0.8660254037844395958, 0.4999999999999982236, 0.000000000000000000 ) ) ;
#21335 = CARTESIAN_POINT ( 'NONE',  ( 1.057460391440397258E-14, -29.16249999999999787, 4.999999999999992006 ) ) ;
#21336 = CARTESIAN_POINT ( 'NONE',  ( 3.999999999999997335, -26.10624999877096997, 11.30940107675849404 ) ) ;
#21337 = CARTESIAN_POINT ( 'NONE',  ( 1.878215178125004048, -5.746835883940462963, 3.478124999385483029 ) ) ;
#21338 = AXIS2_PLACEMENT_3D ( 'NONE', #15860, #17704, #3959 ) ;
#21339 = LINE ( 'NONE', #3421, #21625 ) ;
#21340 = CARTESIAN_POINT ( 'NONE',  ( 3.999999999999942268, -6.690598923241455331, 3.131249998770967213 ) ) ;
#21341 = CARTESIAN_POINT ( 'NONE',  ( 19.78573162020706988, 19.78573162020698462, 12.99999999999999289 ) ) ;
#21342 = ORIENTED_EDGE ( 'NONE', *, *, #7648, .F. ) ;
#21343 = CARTESIAN_POINT ( 'NONE',  ( -16.23990935651735867, -26.52310962334733446, 1.000000000000000000 ) ) ;
#21344 = AXIS2_PLACEMENT_3D ( 'NONE', #12882, #23093, #16827 ) ;
#21345 = ORIENTED_EDGE ( 'NONE', *, *, #12482, .T. ) ;
#21346 = VECTOR ( 'NONE', #21546, 1000.000000000000000 ) ;
#21347 = EDGE_LOOP ( 'NONE', ( #9193, #17521 ) ) ;
#21348 = DIRECTION ( 'NONE',  ( -0.9297764858882532346, -0.3681245526846732008, 0.000000000000000000 ) ) ;
#21349 = ORIENTED_EDGE ( 'NONE', *, *, #16, .F. ) ;
#21350 = CARTESIAN_POINT ( 'NONE',  ( 3.756430356249997882, -27.31562499938548427, 11.16877607737301226 ) ) ;
#21351 = ADVANCED_FACE ( 'NONE', ( #21242 ), #11299, .F. ) ;
#21352 = VERTEX_POINT ( 'NONE', #18908 ) ;
#21353 = DIRECTION ( 'NONE',  ( -0.000000000000000000, -0.000000000000000000, 1.000000000000000000 ) ) ;
#21354 = EDGE_CURVE ( 'NONE', #10560, #2304, #7892, .T. ) ;
#21355 = AXIS2_PLACEMENT_3D ( 'NONE', #8559, #6583, #8678 ) ;
#21356 = ORIENTED_EDGE ( 'NONE', *, *, #4355, .T. ) ;
#21357 = CARTESIAN_POINT ( 'NONE',  ( 2.000000000000000888, 26.27499999999999858, 12.46410161513774817 ) ) ;
#21358 = EDGE_CURVE ( 'NONE', #22500, #1051, #25850, .T. ) ;
#21359 = DIRECTION ( 'NONE',  ( 1.000000000000000000, 0.000000000000000000, 0.000000000000000000 ) ) ;
#21360 = VECTOR ( 'NONE', #22727, 1000.000000000000000 ) ;
#21361 = VECTOR ( 'NONE', #23762, 1000.000000000000000 ) ;
#21362 = ADVANCED_FACE ( 'NONE', ( #13934 ), #4369, .T. ) ;
#21363 = DIRECTION ( 'NONE',  ( 0.000000000000000000, -0.000000000000000000, 1.000000000000000000 ) ) ;
#21364 = CYLINDRICAL_SURFACE ( 'NONE', #23375, 4.000000000000000000 ) ;
#21365 = CARTESIAN_POINT ( 'NONE',  ( 20.77801835412135745, 15.46562359820254784, 6.831223922626973533 ) ) ;
#21366 = CIRCLE ( 'NONE', #8838, 0.5000000000000011102 ) ;
#21367 = DIRECTION ( 'NONE',  ( 0.1253332335643120576, 0.9921147013144768767, 0.000000000000000000 ) ) ;
#21368 = EDGE_CURVE ( 'NONE', #18639, #2848, #3300, .T. ) ;
#21369 = CARTESIAN_POINT ( 'NONE',  ( 4.000000000000003553, 25.48750000000000071, 6.690598923241489970 ) ) ;
#21370 = CARTESIAN_POINT ( 'NONE',  ( 22.39552511608559371, 17.08313036016677700, 11.16877607737301403 ) ) ;
#21371 = CYLINDRICAL_SURFACE ( 'NONE', #2054, 0.4999999999999970024 ) ;
#21372 = AXIS2_PLACEMENT_3D ( 'NONE', #25715, #15534, #13568 ) ;
#21373 = ORIENTED_EDGE ( 'NONE', *, *, #20173, .F. ) ;
#21374 = ORIENTED_EDGE ( 'NONE', *, *, #7539, .F. ) ;
#21375 = CARTESIAN_POINT ( 'NONE',  ( 2.000000000000003553, 27.26874999877097494, 5.535898384862238508 ) ) ;
#21376 = DIRECTION ( 'NONE',  ( -0.000000000000000000, -0.000000000000000000, -1.000000000000000000 ) ) ;
#21377 = ORIENTED_EDGE ( 'NONE', *, *, #4312, .T. ) ;
#21378 = DIRECTION ( 'NONE',  ( 1.000000000000000000, 0.000000000000000000, 0.000000000000000000 ) ) ;
#21379 = CARTESIAN_POINT ( 'NONE',  ( 1.878215178125000939, 28.77812499938548640, 12.25316411605952283 ) ) ;
#21380 = CARTESIAN_POINT ( 'NONE',  ( 0.000000000000000000, 0.000000000000000000, 1.000000000000000000 ) ) ;
#21381 = VERTEX_POINT ( 'NONE', #6334 ) ;
#21382 = ORIENTED_EDGE ( 'NONE', *, *, #2903, .F. ) ;
#21383 = CYLINDRICAL_SURFACE ( 'NONE', #6206, 31.10000000000000142 ) ;
#21384 = AXIS2_PLACEMENT_3D ( 'NONE', #12747, #8438, #8682 ) ;
#21385 = EDGE_CURVE ( 'NONE', #17898, #21186, #739, .T. ) ;
#21386 = LINE ( 'NONE', #13272, #20243 ) ;
#21387 = EDGE_LOOP ( 'NONE', ( #15949, #23537, #11435, #9152 ) ) ;
#21388 = CARTESIAN_POINT ( 'NONE',  ( 4.648177544792955347E-16, 29.33124999877097139, 12.99999999999999289 ) ) ;
#21389 = CARTESIAN_POINT ( 'NONE',  ( 3.735045420075836212E-15, 25.25312499938548783, 4.662447845253954171 ) ) ;
#21390 = CARTESIAN_POINT ( 'NONE',  ( -3.756430356249996549, 29.00312499938548427, 11.16877607737301048 ) ) ;
#21391 = AXIS2_PLACEMENT_3D ( 'NONE', #937, #4852, #6547 ) ;
#21392 = CYLINDRICAL_SURFACE ( 'NONE', #25640, 6.000000000000000888 ) ;
#21393 = CARTESIAN_POINT ( 'NONE',  ( -1.999999999999996669, 26.20000000000000639, 12.46410161513774639 ) ) ;
#21394 = AXIS2_PLACEMENT_3D ( 'NONE', #12159, #24329, #22235 ) ;
#21395 = ADVANCED_FACE ( 'NONE', ( #2021 ), #23863, .F. ) ;
#21396 = CARTESIAN_POINT ( 'NONE',  ( -1.071796769724485454, 27.11740381056766580, 12.99999999999999467 ) ) ;
#21397 = CIRCLE ( 'NONE', #5113, 0.5000000000000006661 ) ;
#21398 = CARTESIAN_POINT ( 'NONE',  ( -30.85476721088022600, 3.897863563850190616, -6.500000000000000000 ) ) ;
#21399 = CARTESIAN_POINT ( 'NONE',  ( -3.756430356249996105, 26.67812499938548498, 6.831223922626973533 ) ) ;
#21400 = CARTESIAN_POINT ( 'NONE',  ( -0.5258040994055174222, -29.99650528990839859, 5.025965267902964939 ) ) ;
#21401 = CARTESIAN_POINT ( 'NONE',  ( 20.56133937125558830, 20.56133937125551370, 13.33755215474602984 ) ) ;
#21402 = CARTESIAN_POINT ( 'NONE',  ( 18.22561351908507277, 20.88181089704437454, 5.746835883940462963 ) ) ;
#21403 = CARTESIAN_POINT ( 'NONE',  ( -31.00322564728510955, 2.451530025009474034, -2.750000000000000000 ) ) ;
#21404 = CARTESIAN_POINT ( 'NONE',  ( -3.756430356250003655, -29.64062499938548356, 8.999999999999992895 ) ) ;
#21405 = CARTESIAN_POINT ( 'NONE',  ( 23.00150435104295354, 19.26045130116930082, 5.988343842124888461 ) ) ;
#21406 = CARTESIAN_POINT ( 'NONE',  ( 19.28854716511979461, 19.28854716511973422, 13.33755215474603162 ) ) ;
#21407 = CARTESIAN_POINT ( 'NONE',  ( 3.469446951953614189E-15, 35.50000000000000711, 8.999999999999992895 ) ) ;
#21408 = ORIENTED_EDGE ( 'NONE', *, *, #9923, .T. ) ;
#21409 = CARTESIAN_POINT ( 'NONE',  ( 19.45547780925145531, 17.93972828139933995, 4.999999999999989342 ) ) ;
#21410 = CARTESIAN_POINT ( 'NONE',  ( -3.756430356249996994, 26.37812499938548783, 8.999999999999992895 ) ) ;
#21411 = CARTESIAN_POINT ( 'NONE',  ( -4.000000000000001776, -26.76249999999999929, 11.30940107675849760 ) ) ;
#21413 = VERTEX_POINT ( 'NONE', #16027 ) ;
#21412 = CARTESIAN_POINT ( 'NONE',  ( -1.878215178124998275, 26.30312499938548854, 5.746835883940462963 ) ) ;
#21414 = CARTESIAN_POINT ( 'NONE',  ( 3.756430356250003211, 27.09062499938548640, 6.831223922626973533 ) ) ;
#21415 = AXIS2_PLACEMENT_3D ( 'NONE', #22763, #14519, #2362 ) ;
#21416 = CARTESIAN_POINT ( 'NONE',  ( 13.02991752792603108, 22.56362157461194329, 20.00001200000000168 ) ) ;
#21417 = CARTESIAN_POINT ( 'NONE',  ( -2.672651547586948120E-15, -27.72812499938548569, 13.33755215474602984 ) ) ;
#21418 = ORIENTED_EDGE ( 'NONE', *, *, #11447, .F. ) ;
#21419 = ORIENTED_EDGE ( 'NONE', *, *, #12831, .F. ) ;
#21420 = CARTESIAN_POINT ( 'NONE',  ( 18.61723445091742235, 23.52487603310535036, 11.00633161724385900 ) ) ;
#21421 = CARTESIAN_POINT ( 'NONE',  ( -3.756430356249996549, 25.36562499938548854, 8.999999999999992895 ) ) ;
#21422 = EDGE_CURVE ( 'NONE', #18350, #7360, #4162, .T. ) ;
#21423 = CARTESIAN_POINT ( 'NONE',  ( -31.00322564728510955, 2.451530025009473590, -6.500000000000000000 ) ) ;
#21424 = VECTOR ( 'NONE', #4622, 1000.000000000000000 ) ;
#21425 = CARTESIAN_POINT ( 'NONE',  ( 2.672651547586948120E-15, -13.33755215474602984, 3.740624999385483651 ) ) ;
#21426 = DIRECTION ( 'NONE',  ( 0.000000000000000000, -1.000000000000000000, 0.000000000000000000 ) ) ;
#21427 = VECTOR ( 'NONE', #24970, 1000.000000000000000 ) ;
#21428 = CARTESIAN_POINT ( 'NONE',  ( 4.000000000000002665, 29.01250000000000284, 11.30940107675849760 ) ) ;
#21429 = PLANE ( 'NONE',  #3395 ) ;
#21430 = CARTESIAN_POINT ( 'NONE',  ( 2.000000000000000888, 28.52500000000000213, 12.46410161513774817 ) ) ;
#21431 = CARTESIAN_POINT ( 'NONE',  ( 1.859271017917182139E-15, 27.08124999877096784, 12.99999999999999289 ) ) ;
#21432 = CARTESIAN_POINT ( 'NONE',  ( 4.000000000000003553, -8.999999999999992895, 18.00000000000000000 ) ) ;
#21433 = CARTESIAN_POINT ( 'NONE',  ( 20.05973549791684718, 17.23130837317058806, 5.535898384862238508 ) ) ;
#21434 = VERTEX_POINT ( 'NONE', #16150 ) ;
#21435 = LINE ( 'NONE', #21172, #13022 ) ;
#21436 = CARTESIAN_POINT ( 'NONE',  ( -3.756430356250004099, -29.34062499938548640, 6.831223922626973533 ) ) ;
#21437 = CARTESIAN_POINT ( 'NONE',  ( -3.756430356249995661, 28.59062499938548640, 6.831223922626973533 ) ) ;
#21438 = CARTESIAN_POINT ( 'NONE',  ( -20.78941499438192508, 22.67092431280617859, 1.000000000000000000 ) ) ;
#21439 = AXIS2_PLACEMENT_3D ( 'NONE', #5392, #1744, #5655 ) ;
#21440 = CARTESIAN_POINT ( 'NONE',  ( 4.000000000000001776, 27.21250000000000213, 11.30940107675849760 ) ) ;
#21441 = CARTESIAN_POINT ( 'NONE',  ( 3.469446951953614189E-15, -8.999999999999992895, 8.000000000000000000 ) ) ;
#21442 = ORIENTED_EDGE ( 'NONE', *, *, #7481, .F. ) ;
#21443 = CARTESIAN_POINT ( 'NONE',  ( 3.469446951953614189E-15, 25.00000000000000000, 8.999999999999992895 ) ) ;
#21444 = CARTESIAN_POINT ( 'NONE',  ( 0.4995657836784084815, 38.49999999999999289, 14.97916666666666075 ) ) ;
#21446 = ORIENTED_EDGE ( 'NONE', *, *, #15787, .F. ) ;
#21445 = CARTESIAN_POINT ( 'NONE',  ( 29.57785765677924061, -9.610428525060996208, 1.000000000000000000 ) ) ;
#21447 = AXIS2_PLACEMENT_3D ( 'NONE', #138, #19859, #1957 ) ;
#21448 = ORIENTED_EDGE ( 'NONE', *, *, #12543, .T. ) ;
#21449 = EDGE_LOOP ( 'NONE', ( #20269, #3081, #25846, #4454 ) ) ;
#21450 = ORIENTED_EDGE ( 'NONE', *, *, #15801, .F. ) ;
#21451 = ORIENTED_EDGE ( 'NONE', *, *, #25751, .T. ) ;
#21452 = DIRECTION ( 'NONE',  ( 1.000000000000000000, 0.000000000000000000, 0.000000000000000000 ) ) ;
#21453 =( BOUNDED_CURVE ( )  B_SPLINE_CURVE ( 2, ( #6383, #14488, #8600, #370, #14373, #18282, #20493, #2591, #14877, #4681, #12660, #2836, #20631, #8341, #20234, #22332, #2713, #10675, #12388, #2330, #20355, #509, #752, #14753, #22731, #4810, #10803, #16852, #10290, #11458, #7155, #11069, #5444, #23355, #15382, #13175, #1017, #7531, #17094, #17358, #19047, #12910, #19309, #19432, #5314, #19170, #25323, #13436, #7015, #7403, #1131, #13047, #21144, #9249, #3104, #22983, #9104, #21406, #25069, #1522, #9491, #5068, #20887, #17474, #21268, #25444, #16970, #15146, #3216, #18933, #24936, #10942, #23114, #5196, #15526, #23231, #11187, #3487, #1265, #8992, #4926, #2974, #17237, #15002, #21025, #25208, #7287, #15263, #13293, #3351, #11326, #1404, #9379, #24003, #17606, #4116, #25708, #3729, #6084, #16042, #8059, #25583, #88, #15652, #21914, #2036, #10004, #5579, #11962, #12095, #23878, #11844, #17999, #14068, #7667, #22034, #11714, #5696, #13810, #1915, #21647 ),
 .UNSPECIFIED., .F., .F. ) 
 B_SPLINE_CURVE_WITH_KNOTS ( ( 3, 2, 2, 2, 2, 2, 2, 2, 2, 2, 2, 2, 2, 2, 2, 2, 2, 2, 2, 2, 2, 2, 2, 2, 2, 2, 2, 2, 2, 2, 2, 2, 2, 2, 2, 2, 2, 2, 2, 2, 2, 2, 2, 2, 2, 2, 2, 2, 2, 2, 2, 2, 2, 2, 2, 2, 2, 2, 2, 2, 3 ),
 ( 0.000000000000000000, 0.01666666666666666644, 0.03333333333333333287, 0.05000000000000000278, 0.06666666666666666574, 0.08333333333333332871, 0.1000000000000000056, 0.1166666666666666685, 0.1333333333333333315, 0.1499999999999999944, 0.1666666666666666574, 0.1833333333333333204, 0.2000000000000000111, 0.2166666666666666741, 0.2333333333333333370, 0.2500000000000000000, 0.2666666666666666630, 0.2833333333333333259, 0.2999999999999999889, 0.3166666666666666519, 0.3333333333333333148, 0.3499999999999999778, 0.3666666666666666408, 0.3833333333333333592, 0.4000000000000000222, 0.4166666666666666852, 0.4333333333333333481, 0.4500000000000000111, 0.4666666666666666741, 0.4833333333333333370, 0.5000000000000000000, 0.5166666666666667185, 0.5333333333333333259, 0.5500000000000000444, 0.5666666666666666519, 0.5833333333333333703, 0.5999999999999999778, 0.6166666666666666963, 0.6333333333333333037, 0.6500000000000000222, 0.6666666666666666297, 0.6833333333333333481, 0.6999999999999999556, 0.7166666666666666741, 0.7333333333333332815, 0.7500000000000000000, 0.7666666666666667185, 0.7833333333333333259, 0.8000000000000000444, 0.8166666666666666519, 0.8333333333333333703, 0.8499999999999999778, 0.8666666666666666963, 0.8833333333333333037, 0.9000000000000000222, 0.9166666666666666297, 0.9333333333333333481, 0.9499999999999999556, 0.9666666666666666741, 0.9833333333333332815, 1.000000000000000000 ),
 .UNSPECIFIED. ) 
 CURVE ( )  GEOMETRIC_REPRESENTATION_ITEM ( )  RATIONAL_B_SPLINE_CURVE ( ( 1.000000000000000000, 0.8660254037844387076, 1.000000000000000000, 0.8660254037844387076, 1.000000000000000000, 0.8660254037844387076, 1.000000000000000000, 0.8660254037844387076, 1.000000000000000000, 0.8660254037844387076, 1.000000000000000000, 0.8660254037844387076, 1.000000000000000000, 0.8660254037844387076, 1.000000000000000000, 0.8660254037844387076, 1.000000000000000000, 0.8660254037844387076, 1.000000000000000000, 0.8660254037844387076, 1.000000000000000000, 0.8660254037844387076, 1.000000000000000000, 0.8660254037844387076, 1.000000000000000000, 0.8660254037844387076, 1.000000000000000000, 0.8660254037844387076, 1.000000000000000000, 0.8660254037844387076, 1.000000000000000000, 0.8660254037844387076, 1.000000000000000000, 0.8660254037844387076, 1.000000000000000000, 0.8660254037844387076, 1.000000000000000000, 0.8660254037844387076, 1.000000000000000000, 0.8660254037844387076, 1.000000000000000000, 0.8660254037844387076, 1.000000000000000000, 0.8660254037844387076, 1.000000000000000000, 0.8660254037844387076, 1.000000000000000000, 0.8660254037844387076, 1.000000000000000000, 0.8660254037844387076, 1.000000000000000000, 0.8660254037844387076, 1.000000000000000000, 0.8660254037844387076, 1.000000000000000000, 0.8660254037844387076, 1.000000000000000000, 0.8660254037844387076, 1.000000000000000000, 0.8660254037844387076, 1.000000000000000000, 0.8660254037844387076, 1.000000000000000000, 0.8660254037844387076, 1.000000000000000000, 0.8660254037844387076, 1.000000000000000000, 0.8660254037844387076, 1.000000000000000000, 0.8660254037844387076, 1.000000000000000000, 0.8660254037844387076, 1.000000000000000000, 0.8660254037844387076, 1.000000000000000000, 0.8660254037844387076, 1.000000000000000000, 0.8660254037844387076, 1.000000000000000000, 0.8660254037844387076, 1.000000000000000000, 0.8660254037844387076, 1.000000000000000000, 0.8660254037844387076, 1.000000000000000000, 0.8660254037844387076, 1.000000000000000000, 0.8660254037844387076, 1.000000000000000000, 0.8660254037844387076, 1.000000000000000000, 0.8660254037844387076, 1.000000000000000000, 0.8660254037844387076, 1.000000000000000000, 0.8660254037844387076, 1.000000000000000000, 0.8660254037844387076, 1.000000000000000000, 0.8660254037844387076, 1.000000000000000000, 0.8660254037844387076, 1.000000000000000000, 0.8660254037844387076, 1.000000000000000000, 0.8660254037844387076, 1.000000000000000000, 0.8660254037844387076, 1.000000000000000000, 0.8660254037844387076, 1.000000000000000000, 0.8660254037844387076, 1.000000000000000000, 0.8660254037844387076, 1.000000000000000000, 0.8660254037844387076, 1.000000000000000000, 0.8660254037844387076, 1.000000000000000000, 0.8660254037844387076, 1.000000000000000000 ) ) 
 REPRESENTATION_ITEM ( '' )  );
#21454 = CARTESIAN_POINT ( 'NONE',  ( -3.051911138222374031, 38.91143067427094593, 13.68207702368797918 ) ) ;
#21455 = ADVANCED_FACE ( 'NONE', ( #5948 ), #20187, .T. ) ;
#21456 = DIRECTION ( 'NONE',  ( 0.9510565162951586382, 0.3090169943749320192, 0.000000000000000000 ) ) ;
#21457 =( BOUNDED_CURVE ( )  B_SPLINE_CURVE ( 2, ( #8231, #16210, #4796, #24178, #6266, #22225, #4310, #8360, #12773 ),
 .UNSPECIFIED., .F., .F. ) 
 B_SPLINE_CURVE_WITH_KNOTS ( ( 3, 2, 2, 2, 3 ),
 ( 0.8250000000000000666, 0.8333333333333333703, 0.8499999999999999778, 0.8666666666666666963, 0.8750000000000000000 ),
 .UNSPECIFIED. ) 
 CURVE ( )  GEOMETRIC_REPRESENTATION_ITEM ( )  RATIONAL_B_SPLINE_CURVE ( ( 0.9330127018922194093, 0.9330127018922198534, 1.000000000000000000, 0.8660254037844387076, 1.000000000000000000, 0.8660254037844387076, 1.000000000000000000, 0.9330127018922194093, 0.9330127018922194093 ) ) 
 REPRESENTATION_ITEM ( '' )  );
#21458 = ADVANCED_FACE ( 'NONE', ( #321 ), #2287, .T. ) ;
#21459 = CARTESIAN_POINT ( 'NONE',  ( 1.878215178125000939, -12.25316411605952283, 3.665624999385483473 ) ) ;
#21460 = CARTESIAN_POINT ( 'NONE',  ( 4.000000000000003553, -8.999999999999992895, 2.193749998770967213 ) ) ;
#21461 = EDGE_CURVE ( 'NONE', #4288, #2145, #12080, .T. ) ;
#21462 = CARTESIAN_POINT ( 'NONE',  ( -3.756430356249997882, 28.21562499938548285, 11.16877607737301226 ) ) ;
#21463 = AXIS2_PLACEMENT_3D ( 'NONE', #14596, #16449, #22440 ) ;
#21464 = CARTESIAN_POINT ( 'NONE',  ( -30.04913349766228592, -5.827558883615738594, -6.500000000000000000 ) ) ;
#21465 = CARTESIAN_POINT ( 'NONE',  ( 21.21320343559646915, 21.21320343559638744, 12.99999999999999289 ) ) ;
#21466 = CARTESIAN_POINT ( 'NONE',  ( -1.999999999999995781, -5.535898384862237620, 2.399999999999999467 ) ) ;
#21467 = CARTESIAN_POINT ( 'NONE',  ( -1.071796769724494336, -25.75134618820330346, 12.99999999999999467 ) ) ;
#21469 = EDGE_CURVE ( 'NONE', #24918, #23707, #14450, .T. ) ;
#21468 = DIRECTION ( 'NONE',  ( 0.000000000000000000, 0.000000000000000000, -1.000000000000000000 ) ) ;
#21470 = CARTESIAN_POINT ( 'NONE',  ( 4.000000000000005329, 27.73750000000000782, 6.690598923241489970 ) ) ;
#21471 = CARTESIAN_POINT ( 'NONE',  ( -2.620986760973688460E-15, -26.18124999877096926, 13.61880215351699874 ) ) ;
#21472 = CARTESIAN_POINT ( 'NONE',  ( 0.000000000000000000, 0.000000000000000000, -6.500000000000000000 ) ) ;
#21473 = DIRECTION ( 'NONE',  ( 1.000000000000000000, 0.000000000000000000, 0.000000000000000000 ) ) ;
#21474 = CYLINDRICAL_SURFACE ( 'NONE', #10795, 4.000000000000000000 ) ;
#21475 = DIRECTION ( 'NONE',  ( 1.000000000000000000, 0.000000000000000000, 0.000000000000000000 ) ) ;
#21476 = VERTEX_POINT ( 'NONE', #10126 ) ;
#21477 = CYLINDRICAL_SURFACE ( 'NONE', #12096, 31.10000000000000142 ) ;
#21478 = VERTEX_POINT ( 'NONE', #4491 ) ;
#21479 = ORIENTED_EDGE ( 'NONE', *, *, #4897, .T. ) ;
#21480 = CYLINDRICAL_SURFACE ( 'NONE', #21645, 31.10000000000000142 ) ;
#21481 =( GEOMETRIC_REPRESENTATION_CONTEXT ( 3 ) GLOBAL_UNCERTAINTY_ASSIGNED_CONTEXT ( ( #12807 ) ) GLOBAL_UNIT_ASSIGNED_CONTEXT ( ( #8621, #16989, #23003 ) ) REPRESENTATION_CONTEXT ( 'NONE', 'WORKASPACE' ) );
#21482 = EDGE_LOOP ( 'NONE', ( #10078, #5619, #15330, #10467 ) ) ;
#21483 = CARTESIAN_POINT ( 'NONE',  ( -3.756430356250004099, -28.44062499938548783, 6.831223922626973533 ) ) ;
#21484 = ORIENTED_EDGE ( 'NONE', *, *, #19509, .F. ) ;
#21485 = CARTESIAN_POINT ( 'NONE',  ( -0.5000000000000000000, 0.000000000000000000, 20.00000000000000000 ) ) ;
#21486 = ORIENTED_EDGE ( 'NONE', *, *, #18524, .F. ) ;
#21487 = CARTESIAN_POINT ( 'NONE',  ( 4.000000000000003553, 26.83749999999999503, 6.690598923241489970 ) ) ;
#21488 = LINE ( 'NONE', #23443, #13083 ) ;
#21489 = CYLINDRICAL_SURFACE ( 'NONE', #25549, 4.000000000000000000 ) ;
#21490 = PRODUCT_RELATED_PRODUCT_CATEGORY ( 'part', '', ( #8177 ) ) ;
#21491 = CARTESIAN_POINT ( 'NONE',  ( -3.897863563849436552, 30.85476721088031482, -6.500000000000000000 ) ) ;
#21492 = CARTESIAN_POINT ( 'NONE',  ( 20.00449278107117834, 20.00449278107111084, 13.33755215474602984 ) ) ;
#21493 = CARTESIAN_POINT ( 'NONE',  ( -1.071796769724487675, 27.32634618820330630, 4.999999999999992895 ) ) ;
#21494 = EDGE_CURVE ( 'NONE', #16478, #7351, #16278, .T. ) ;
#21495 = CARTESIAN_POINT ( 'NONE',  ( -3.999999999999996003, 25.63749999999999929, 6.690598923241487306 ) ) ;
#21496 = EDGE_CURVE ( 'NONE', #3018, #14914, #8432, .T. ) ;
#21497 = FACE_OUTER_BOUND ( 'NONE', #20365, .T. ) ;
#21498 = ORIENTED_EDGE ( 'NONE', *, *, #8109, .T. ) ;
#21499 = ORIENTED_EDGE ( 'NONE', *, *, #12825, .F. ) ;
#21500 = CARTESIAN_POINT ( 'NONE',  ( 1.999999999999998224, 26.66874999877097352, 12.46410161513774817 ) ) ;
#21501 = EDGE_LOOP ( 'NONE', ( #10873, #1828, #25218, #16257 ) ) ;
#21502 = CARTESIAN_POINT ( 'NONE',  ( 1.071796769724495668, 26.25759618943233065, 12.99999999999999112 ) ) ;
#21503 = CARTESIAN_POINT ( 'NONE',  ( 3.735045420075836212E-15, 28.06562499938548427, 4.662447845253954171 ) ) ;
#21504 = CARTESIAN_POINT ( 'NONE',  ( -3.959305671612554781E-15, -30.00000000000000355, 12.99999999999999289 ) ) ;
#21505 = VERTEX_POINT ( 'NONE', #12467 ) ;
#21506 = ORIENTED_EDGE ( 'NONE', *, *, #23952, .T. ) ;
#21507 = CARTESIAN_POINT ( 'NONE',  ( 4.000000000000001776, 25.00000000000000000, 8.999999999999992895 ) ) ;
#21508 = ORIENTED_EDGE ( 'NONE', *, *, #17270, .T. ) ;
#21509 = FACE_OUTER_BOUND ( 'NONE', #2495, .T. ) ;
#21510 = CARTESIAN_POINT ( 'NONE',  ( 3.756430356250002323, 28.25312499938548783, 11.16877607737301403 ) ) ;
#21511 = CARTESIAN_POINT ( 'NONE',  ( 6.009258394948636914E-15, 27.36250000000000782, 4.381197846482986158 ) ) ;
#21512 = EDGE_CURVE ( 'NONE', #9321, #19215, #24107, .T. ) ;
#21513 = CARTESIAN_POINT ( 'NONE',  ( 3.735045420075836212E-15, 28.40312499938548640, 4.662447845253954171 ) ) ;
#21514 = CARTESIAN_POINT ( 'NONE',  ( -12.74173596767398742, -28.14012133169310559, -6.500000000000000000 ) ) ;
#21515 = EDGE_CURVE ( 'NONE', #13703, #14349, #22933, .T. ) ;
#21516 = LINE ( 'NONE', #5188, #2994 ) ;
#21517 = CARTESIAN_POINT ( 'NONE',  ( 3.756430356250003211, 27.42812499938548143, 6.831223922626973533 ) ) ;
#21518 = AXIS2_PLACEMENT_3D ( 'NONE', #2454, #18416, #6252 ) ;
#21519 = DIRECTION ( 'NONE',  ( 0.000000000000000000, 0.000000000000000000, 1.000000000000000000 ) ) ;
#21520 = CARTESIAN_POINT ( 'NONE',  ( 17.43018215624843847, 20.25860928099455904, 12.46410161513774639 ) ) ;
#21521 = CARTESIAN_POINT ( 'NONE',  ( 22.07732706455164617, 16.76493230863282591, 11.16877607737301226 ) ) ;
#21522 = LINE ( 'NONE', #13289, #472 ) ;
#21523 = FACE_OUTER_BOUND ( 'NONE', #12658, .T. ) ;
#21524 = CARTESIAN_POINT ( 'NONE',  ( 3.469446951953614189E-15, -8.999999999999992895, 8.000000000000000000 ) ) ;
#21525 = CARTESIAN_POINT ( 'NONE',  ( 3.000000000000003997, -8.999999999999992895, 18.00000000000000000 ) ) ;
#21526 = CARTESIAN_POINT ( 'NONE',  ( 24.86329371854761305, -18.68225429291740269, -2.750000000000000000 ) ) ;
#21527 = ORIENTED_EDGE ( 'NONE', *, *, #18201, .T. ) ;
#21528 = CARTESIAN_POINT ( 'NONE',  ( -3.897863563850083146, -30.85476721088024021, -6.500000000000000000 ) ) ;
#21529 = CARTESIAN_POINT ( 'NONE',  ( -4.000000000000003553, -26.83749999999999503, 6.690598923241489970 ) ) ;
#21531 = EDGE_LOOP ( 'NONE', ( #3494, #1099, #11849, #4258 ) ) ;
#21530 = DIRECTION ( 'NONE',  ( 0.000000000000000000, 0.000000000000000000, 1.000000000000000000 ) ) ;
#21532 = CARTESIAN_POINT ( 'NONE',  ( -1.878215178124995832, 25.40312499938548640, 5.746835883940462963 ) ) ;
#21533 = CARTESIAN_POINT ( 'NONE',  ( 4.000000000000003553, -8.999999999999992895, 0.4499999999999990119 ) ) ;
#21534 = CARTESIAN_POINT ( 'NONE',  ( -26.00000000000000355, -1.592040838891558504E-15, 20.00000599999999906 ) ) ;
#21535 = CARTESIAN_POINT ( 'NONE',  ( 3.756430356249997882, -29.45312499938548356, 11.16877607737301226 ) ) ;
#21536 = CIRCLE ( 'NONE', #10245, 31.10000000000000142 ) ;
#21537 = ORIENTED_EDGE ( 'NONE', *, *, #22909, .F. ) ;
#21538 = ORIENTED_EDGE ( 'NONE', *, *, #23843, .F. ) ;
#21539 = CARTESIAN_POINT ( 'NONE',  ( -2.672651547586948120E-15, -25.59062499938548640, 13.33755215474603162 ) ) ;
#21540 = CARTESIAN_POINT ( 'NONE',  ( 1.878215178125001605, 29.22812499938549280, 12.25316411605952283 ) ) ;
#21541 = CARTESIAN_POINT ( 'NONE',  ( -1.878215178124995832, -5.746835883940462963, 0.2906249993854838065 ) ) ;
#21542 = CARTESIAN_POINT ( 'NONE',  ( -1.878215178124998497, -12.25316411605951927, 3.253124999385483829 ) ) ;
#21543 =( NAMED_UNIT ( * ) SI_UNIT ( $, .STERADIAN. ) SOLID_ANGLE_UNIT ( ) );
#21544 = EDGE_CURVE ( 'NONE', #19408, #961, #15956, .T. ) ;
#21545 = CARTESIAN_POINT ( 'NONE',  ( -3.469446951953614189E-15, -30.00000000000000355, 8.999999999999992895 ) ) ;
#21546 = DIRECTION ( 'NONE',  ( 0.000000000000000000, 0.000000000000000000, -1.000000000000000000 ) ) ;
#21547 = FACE_OUTER_BOUND ( 'NONE', #9417, .T. ) ;
#21548 =( BOUNDED_CURVE ( )  B_SPLINE_CURVE ( 2, ( #8952, #7715, #5013, #25155, #970, #17182, #5625, #20976, #15697 ),
 .UNSPECIFIED., .F., .F. ) 
 B_SPLINE_CURVE_WITH_KNOTS ( ( 3, 2, 2, 2, 3 ),
 ( 0.9250000000000000444, 0.9333333333333333481, 0.9499999999999999556, 0.9666666666666666741, 0.9749999999999999778 ),
 .UNSPECIFIED. ) 
 CURVE ( )  GEOMETRIC_REPRESENTATION_ITEM ( )  RATIONAL_B_SPLINE_CURVE ( ( 0.9330127018922194093, 0.9330127018922198534, 1.000000000000000000, 0.8660254037844387076, 1.000000000000000000, 0.8660254037844387076, 1.000000000000000000, 0.9330127018922194093, 0.9330127018922194093 ) ) 
 REPRESENTATION_ITEM ( '' )  );
#21549 = CARTESIAN_POINT ( 'NONE',  ( -3.063240906311874401, -29.84319947910909931, 11.57226653943513028 ) ) ;
#21550 = CARTESIAN_POINT ( 'NONE',  ( -3.999999999999996447, 26.96874999877096712, 8.999999999999992895 ) ) ;
#21551 = CARTESIAN_POINT ( 'NONE',  ( 0.5000000000000000000, 0.8660254037844387076, 19.50000000000000000 ) ) ;
#21552 = CARTESIAN_POINT ( 'NONE',  ( 21.73911410323489690, 16.08225985374244615, 8.999999999999992895 ) ) ;
#21553 = ORIENTED_EDGE ( 'NONE', *, *, #11089, .F. ) ;
#21554 = CARTESIAN_POINT ( 'NONE',  ( 5.706339097771728319, 38.63519838069890966, 7.645898033751371337 ) ) ;
#21555 = CARTESIAN_POINT ( 'NONE',  ( -3.756430356250003655, -29.75312499938548783, 8.999999999999992895 ) ) ;
#21556 = CARTESIAN_POINT ( 'NONE',  ( -3.756430356249997882, 28.66562499938548569, 11.16877607737301226 ) ) ;
#21557 = ADVANCED_FACE ( 'NONE', ( #24628 ), #22686, .T. ) ;
#21558 = CARTESIAN_POINT ( 'NONE',  ( 21.21320343559646915, 21.21320343559638744, 8.999999999999992895 ) ) ;
#21559 = CARTESIAN_POINT ( 'NONE',  ( 3.048878893044081551, 38.61087488181073724, 14.03846737935104549 ) ) ;
#21560 = ORIENTED_EDGE ( 'NONE', *, *, #13785, .T. ) ;
#21561 = CARTESIAN_POINT ( 'NONE',  ( 0.000000000000000000, 0.000000000000000000, -6.500000000000000000 ) ) ;
#21562 = CARTESIAN_POINT ( 'NONE',  ( -6.317933499823532806, -30.45149776762725580, 1.000000000000000000 ) ) ;
#21564 = ORIENTED_EDGE ( 'NONE', *, *, #6324, .F. ) ;
#21563 = CARTESIAN_POINT ( 'NONE',  ( 28.72825533807133169, 11.91206721063041485, -6.500000000000000000 ) ) ;
#21565 = EDGE_CURVE ( 'NONE', #22574, #12137, #711, .T. ) ;
#21566 = VERTEX_POINT ( 'NONE', #24772 ) ;
#21567 = VERTEX_POINT ( 'NONE', #2792 ) ;
#21568 = VERTEX_POINT ( 'NONE', #10757 ) ;
#21569 = ORIENTED_EDGE ( 'NONE', *, *, #18499, .F. ) ;
#21570 = LINE ( 'NONE', #3649, #9300 ) ;
#21571 = CARTESIAN_POINT ( 'NONE',  ( -4.000000000000001776, -28.05624999877096570, 11.30940107675849760 ) ) ;
#21572 = CARTESIAN_POINT ( 'NONE',  ( 12.78762572734057024, 28.34936733434201273, -2.750000000000000000 ) ) ;
#21573 = CARTESIAN_POINT ( 'NONE',  ( 1.878215178125003382, 25.66562499938548214, 5.746835883940462963 ) ) ;
#21574 = CARTESIAN_POINT ( 'NONE',  ( -3.756430356249995661, -6.831223922626973533, 2.128124999385482052 ) ) ;
#21575 = CARTESIAN_POINT ( 'NONE',  ( 4.000000000000001776, -11.30940107675849760, 3.056249998770964371 ) ) ;
#21576 = LINE ( 'NONE', #5500, #17694 ) ;
#21577 = CARTESIAN_POINT ( 'NONE',  ( 1.878215178125004048, 28.92812499938548854, 5.746835883940462963 ) ) ;
#21578 = CARTESIAN_POINT ( 'NONE',  ( 0.000000000000000000, 0.000000000000000000, -6.500000000000000000 ) ) ;
#21579 = CYLINDRICAL_SURFACE ( 'NONE', #9686, 0.5000000000000004441 ) ;
#21580 = CARTESIAN_POINT ( 'NONE',  ( 3.752267015613588906E-15, -4.381197846482986158, 1.012499999999998401 ) ) ;
#21581 = CARTESIAN_POINT ( 'NONE',  ( 3.469446951953614189E-15, 46.00000000000000000, 8.999999999999992895 ) ) ;
#21582 = DIRECTION ( 'NONE',  ( 1.000000000000000000, 0.000000000000000000, 0.000000000000000000 ) ) ;
#21583 = CARTESIAN_POINT ( 'NONE',  ( 3.137519842735244810E-15, -27.30624999877096926, 4.999999999999991118 ) ) ;
#21584 = CARTESIAN_POINT ( 'NONE',  ( 1.999999999999998224, -27.49374999877096926, 12.46410161513774639 ) ) ;
#21585 = CARTESIAN_POINT ( 'NONE',  ( 1.878215178125004048, 28.02812499938548640, 5.746835883940462963 ) ) ;
#21586 = CIRCLE ( 'NONE', #20321, 31.10000000000000142 ) ;
#21587 = CYLINDRICAL_SURFACE ( 'NONE', #19951, 31.10000000000000142 ) ;
#21588 = ADVANCED_FACE ( 'NONE', ( #8679 ), #14837, .T. ) ;
#21589 = CARTESIAN_POINT ( 'NONE',  ( -3.999999999999996447, -8.999999999999992895, 18.00000000000000000 ) ) ;
#21590 = LINE ( 'NONE', #17684, #19745 ) ;
#21591 = ORIENTED_EDGE ( 'NONE', *, *, #1365, .T. ) ;
#21592 = CARTESIAN_POINT ( 'NONE',  ( 1.071796769724492338, 28.50759618943233775, 12.99999999999999467 ) ) ;
#21593 = VERTEX_POINT ( 'NONE', #11029 ) ;
#21594 = EDGE_CURVE ( 'NONE', #21679, #3647, #905, .T. ) ;
#21595 = EDGE_LOOP ( 'NONE', ( #15742, #16297, #20674, #13684 ) ) ;
#21596 = DIRECTION ( 'NONE',  ( 0.3090169943749456194, -0.9510565162951541973, 0.000000000000000000 ) ) ;
#21597 = VERTEX_POINT ( 'NONE', #8956 ) ;
#21598 = ADVANCED_FACE ( 'NONE', ( #24899 ), #3060, .T. ) ;
#21599 = CARTESIAN_POINT ( 'NONE',  ( -1.878215178125000939, -27.42812499938548498, 12.25316411605952283 ) ) ;
#21600 = ORIENTED_EDGE ( 'NONE', *, *, #6718, .F. ) ;
#21601 = DIRECTION ( 'NONE',  ( 0.000000000000000000, 0.000000000000000000, 1.000000000000000000 ) ) ;
#21602 =( BOUNDED_CURVE ( )  B_SPLINE_CURVE ( 2, ( #3423, #17033, #23295, #9439, #15460, #5381, #23051, #17420, #16916 ),
 .UNSPECIFIED., .F., .F. ) 
 B_SPLINE_CURVE_WITH_KNOTS ( ( 3, 2, 2, 2, 3 ),
 ( 0.1749999999999999889, 0.1833333333333333204, 0.2000000000000000111, 0.2166666666666666741, 0.2250000000000000056 ),
 .UNSPECIFIED. ) 
 CURVE ( )  GEOMETRIC_REPRESENTATION_ITEM ( )  RATIONAL_B_SPLINE_CURVE ( ( 0.9330127018922194093, 0.9330127018922194093, 1.000000000000000000, 0.8660254037844387076, 1.000000000000000000, 0.8660254037844387076, 1.000000000000000000, 0.9330127018922194093, 0.9330127018922194093 ) ) 
 REPRESENTATION_ITEM ( '' )  );
#21603 = ORIENTED_EDGE ( 'NONE', *, *, #769, .F. ) ;
#21604 = EDGE_CURVE ( 'NONE', #20539, #21627, #2892, .T. ) ;
#21605 = CARTESIAN_POINT ( 'NONE',  ( -3.999999999999996003, 26.08750000000000213, 6.690598923241487306 ) ) ;
#21606 = CARTESIAN_POINT ( 'NONE',  ( 21.65113613650327196, -22.32573188046928436, 1.000000000000000000 ) ) ;
#21607 = CARTESIAN_POINT ( 'NONE',  ( 1.878215178125004048, -5.746835883940462963, 0.3281249993854831737 ) ) ;
#21608 = CARTESIAN_POINT ( 'NONE',  ( -1.999999999999998224, 25.75000000000000711, 12.46410161513774639 ) ) ;
#21609 = CARTESIAN_POINT ( 'NONE',  ( 17.24222938593383248, 22.55462414185250353, 6.831223922626973533 ) ) ;
#21610 = EDGE_CURVE ( 'NONE', #7673, #1524, #25021, .T. ) ;
#21611 = CARTESIAN_POINT ( 'NONE',  ( -3.999999999999996003, 28.33750000000000213, 6.690598923241487306 ) ) ;
#21612 = CARTESIAN_POINT ( 'NONE',  ( -1.071796769724493448, 29.18259618943233136, 4.999999999999995559 ) ) ;
#21613 = LINE ( 'NONE', #13773, #497 ) ;
#21614 = ORIENTED_EDGE ( 'NONE', *, *, #12648, .F. ) ;
#21615 = ORIENTED_EDGE ( 'NONE', *, *, #10760, .F. ) ;
#21616 = CARTESIAN_POINT ( 'NONE',  ( -3.999999999999996447, 29.18124999877097281, 6.690598923241487306 ) ) ;
#21617 = ORIENTED_EDGE ( 'NONE', *, *, #1508, .F. ) ;
#21618 = CYLINDRICAL_SURFACE ( 'NONE', #4573, 4.000000000000000000 ) ;
#21619 =( REPRESENTATION_RELATIONSHIP ('NONE','NONE', #25031, #8162 ) REPRESENTATION_RELATIONSHIP_WITH_TRANSFORMATION ( #10610 )SHAPE_REPRESENTATION_RELATIONSHIP( ) );
#21620 = CARTESIAN_POINT ( 'NONE',  ( -3.999999999999998224, 29.27500000000000568, 8.999999999999992895 ) ) ;
#21621 = CARTESIAN_POINT ( 'NONE',  ( 1.626862140677534194E-14, 27.98124999877096997, 12.99999999999999289 ) ) ;
#21622 = VERTEX_POINT ( 'NONE', #23072 ) ;
#21623 = EDGE_CURVE ( 'NONE', #19911, #25487, #13133, .T. ) ;
#21624 = ORIENTED_EDGE ( 'NONE', *, *, #8933, .T. ) ;
#21625 = VECTOR ( 'NONE', #5895, 1000.000000000000000 ) ;
#21626 = CARTESIAN_POINT ( 'NONE',  ( 0.5000000000000000000, -2.999999999999999556, 20.00000000000000000 ) ) ;
#21627 = VERTEX_POINT ( 'NONE', #8560 ) ;
#21628 = EDGE_CURVE ( 'NONE', #18048, #161, #13356, .T. ) ;
#21629 = CARTESIAN_POINT ( 'NONE',  ( -19.82388608118446527, -23.96296185032687376, -6.500000000000000000 ) ) ;
#21630 = DIRECTION ( 'NONE',  ( -0.000000000000000000, -0.000000000000000000, 1.000000000000000000 ) ) ;
#21631 = CARTESIAN_POINT ( 'NONE',  ( 1.878215178125001605, 28.66562499938549280, 12.25316411605952283 ) ) ;
#21632 = EDGE_CURVE ( 'NONE', #7170, #16109, #15733, .T. ) ;
#21633 = AXIS2_PLACEMENT_3D ( 'NONE', #2477, #20659, #6407 ) ;
#21634 = CARTESIAN_POINT ( 'NONE',  ( 19.66640735175089105, 19.66640735175081289, 4.999999999999992006 ) ) ;
#21635 = CARTESIAN_POINT ( 'NONE',  ( -3.999999999999996447, 27.96250000000000568, 11.30940107675849404 ) ) ;
#21636 = CARTESIAN_POINT ( 'NONE',  ( 3.735045420075836212E-15, 25.70312499938548001, 4.662447845253954171 ) ) ;
#21637 = CYLINDRICAL_SURFACE ( 'NONE', #15464, 0.5000000000000004441 ) ;
#21638 = FACE_OUTER_BOUND ( 'NONE', #14965, .T. ) ;
#21639 = AXIS2_PLACEMENT_3D ( 'NONE', #11876, #3637, #1944 ) ;
#21640 = DIRECTION ( 'NONE',  ( -0.000000000000000000, -1.000000000000000000, 0.000000000000000000 ) ) ;
#21641 = CARTESIAN_POINT ( 'NONE',  ( 18.39361514561510447, 18.39361514561503341, 4.381197846482986158 ) ) ;
#21642 = CARTESIAN_POINT ( 'NONE',  ( 17.56042743746777646, 22.87282219338644751, 6.831223922626973533 ) ) ;
#21643 = CARTESIAN_POINT ( 'NONE',  ( -3.677829432474411853, -29.77381621822422275, 10.59017455026297405 ) ) ;
#21644 = CARTESIAN_POINT ( 'NONE',  ( 3.756430356250004099, 29.22812499938548925, 6.831223922626973533 ) ) ;
#21646 = CARTESIAN_POINT ( 'NONE',  ( 22.87163432207205460, 19.41484867808718207, 5.822820249163556561 ) ) ;
#21645 = AXIS2_PLACEMENT_3D ( 'NONE', #19881, #5904, #5521 ) ;
#21647 = CARTESIAN_POINT ( 'NONE',  ( 23.61528431363239022, 18.30288955771356640, 8.999999999999992895 ) ) ;
#21648 = CARTESIAN_POINT ( 'NONE',  ( -3.469446951953614189E-15, -30.00000000000000355, 8.999999999999992895 ) ) ;
#21649 = VECTOR ( 'NONE', #3632, 1000.000000000000000 ) ;
#21650 = ORIENTED_EDGE ( 'NONE', *, *, #22050, .T. ) ;
#21651 = CARTESIAN_POINT ( 'NONE',  ( 4.000000000000003553, 26.29374999877096997, 8.999999999999992895 ) ) ;
#21652 = CARTESIAN_POINT ( 'NONE',  ( -2.000000000000003997, -25.52500000000000213, 5.535898384862238508 ) ) ;
#21654 = ORIENTED_EDGE ( 'NONE', *, *, #13200, .T. ) ;
#21653 = CARTESIAN_POINT ( 'NONE',  ( -1.878215178124998275, 26.00312499938549493, 12.25316411605951927 ) ) ;
#21655 = CARTESIAN_POINT ( 'NONE',  ( -3.756430356249996994, 28.62812499938548427, 8.999999999999992895 ) ) ;
#21656 = CARTESIAN_POINT ( 'NONE',  ( 3.897863563849872204, 30.85476721088026508, 1.000000000000000000 ) ) ;
#21657 = CARTESIAN_POINT ( 'NONE',  ( 25.16843286583313599, 6.741346781237259833, 20.00001200000000523 ) ) ;
#21658 = DIRECTION ( 'NONE',  ( 1.000000000000000000, 0.000000000000000000, 0.000000000000000000 ) ) ;
#21659 = EDGE_LOOP ( 'NONE', ( #11137, #14944, #15770 ) ) ;
#21660 = VERTEX_POINT ( 'NONE', #23448 ) ;
#21661 = ADVANCED_FACE ( 'NONE', ( #23695 ), #5776, .F. ) ;
#21662 = SURFACE_STYLE_USAGE ( .BOTH. , #10147 ) ;
#21663 = CARTESIAN_POINT ( 'NONE',  ( -3.756430356250000546, 26.30312499938548854, 11.16877607737301226 ) ) ;
#21664 = EDGE_CURVE ( 'NONE', #2083, #18610, #16693, .T. ) ;
#21665 = AXIS2_PLACEMENT_3D ( 'NONE', #13260, #3189, #18078 ) ;
#21666 = VECTOR ( 'NONE', #21640, 1000.000000000000000 ) ;
#21667 = CARTESIAN_POINT ( 'NONE',  ( -1.878215178124998497, -12.25316411605951927, 3.140624999385482230 ) ) ;
#21668 = EDGE_CURVE ( 'NONE', #5730, #5871, #15260, .T. ) ;
#21669 = CIRCLE ( 'NONE', #25018, 0.4999999999999986122 ) ;
#21670 = AXIS2_PLACEMENT_3D ( 'NONE', #12948, #14518, #12417 ) ;
#21671 = CARTESIAN_POINT ( 'NONE',  ( 3.401318489841097747, 30.91344420362547396, -6.500000000000000000 ) ) ;
#21672 = DIRECTION ( 'NONE',  ( -0.000000000000000000, 0.000000000000000000, 1.000000000000000000 ) ) ;
#21673 = CARTESIAN_POINT ( 'NONE',  ( 10.98232076577222038, 29.09636799667079288, 1.000000000000000000 ) ) ;
#21674 = DIRECTION ( 'NONE',  ( -0.000000000000000000, -0.000000000000000000, -1.000000000000000000 ) ) ;
#21675 = DIRECTION ( 'NONE',  ( 0.000000000000000000, 0.000000000000000000, 1.000000000000000000 ) ) ;
#21676 = CARTESIAN_POINT ( 'NONE',  ( -0.7500000000000001110, 1.299038105676658450, 17.69999999999999929 ) ) ;
#21677 = CARTESIAN_POINT ( 'NONE',  ( -3.110308778861380574, 31.50000000000000000, 3.869115154270378110 ) ) ;
#21678 = CARTESIAN_POINT ( 'NONE',  ( 15.60496277644160124, 21.26181702593391876, 8.999999999999992895 ) ) ;
#21679 = VERTEX_POINT ( 'NONE', #11417 ) ;
#21680 = CARTESIAN_POINT ( 'NONE',  ( -9.610428525061097460, -29.57785765677920509, -6.500000000000000000 ) ) ;
#21681 = CARTESIAN_POINT ( 'NONE',  ( -1.878215178125004048, -29.37812499938548783, 5.746835883940462963 ) ) ;
#21682 = CARTESIAN_POINT ( 'NONE',  ( 3.756430356250002323, 26.56562499938548427, 11.16877607737301226 ) ) ;
#21683 = CARTESIAN_POINT ( 'NONE',  ( 21.14249275747780032, 15.48563850798535491, 8.999999999999992895 ) ) ;
#21684 = VECTOR ( 'NONE', #9148, 1000.000000000000000 ) ;
#21685 = CARTESIAN_POINT ( 'NONE',  ( -3.999999999999996447, 29.18124999877097281, 6.690598923241487306 ) ) ;
#21686 = CARTESIAN_POINT ( 'NONE',  ( 3.296389899763111586, 38.99989214654019776, 13.40352862988387095 ) ) ;
#21687 = ORIENTED_EDGE ( 'NONE', *, *, #24522, .T. ) ;
#21688 = LINE ( 'NONE', #9793, #13853 ) ;
#21689 = CARTESIAN_POINT ( 'NONE',  ( -5.438844394475538024, 38.59945611884848660, 6.711898833373152407 ) ) ;
#21691 = VERTEX_POINT ( 'NONE', #17565 ) ;
#21690 = CARTESIAN_POINT ( 'NONE',  ( 1.999999999999995781, -26.44374999877096855, 5.535898384862237620 ) ) ;
#21692 = AXIS2_PLACEMENT_3D ( 'NONE', #14420, #4072, #4207 ) ;
#21693 = ORIENTED_EDGE ( 'NONE', *, *, #5556, .T. ) ;
#21695 = ORIENTED_EDGE ( 'NONE', *, *, #17500, .T. ) ;
#21694 = CIRCLE ( 'NONE', #405, 0.5000000000000006661 ) ;
#21696 = VERTEX_POINT ( 'NONE', #13762 ) ;
#21697 = ORIENTED_EDGE ( 'NONE', *, *, #19307, .T. ) ;
#21698 = FACE_OUTER_BOUND ( 'NONE', #6841, .T. ) ;
#21699 = CARTESIAN_POINT ( 'NONE',  ( -3.508499826075089700, 38.91217497027906802, 13.34949135706027690 ) ) ;
#21700 = ADVANCED_FACE ( 'NONE', ( #15342 ), #21220, .T. ) ;
#21701 = CIRCLE ( 'NONE', #9582, 0.4999999999999992784 ) ;
#21702 =( NAMED_UNIT ( * ) SI_UNIT ( $, .STERADIAN. ) SOLID_ANGLE_UNIT ( ) );
#21703 = DIRECTION ( 'NONE',  ( 1.000000000000000000, 0.000000000000000000, 0.000000000000000000 ) ) ;
#21704 = AXIS2_PLACEMENT_3D ( 'NONE', #3207, #3475, #5569 ) ;
#21705 = AXIS2_PLACEMENT_3D ( 'NONE', #17100, #15008, #17243 ) ;
#21706 = CARTESIAN_POINT ( 'NONE',  ( -3.756430356249997882, -11.16877607737301226, 2.203124999385479565 ) ) ;
#21707 = CARTESIAN_POINT ( 'NONE',  ( 1.878215178125004048, -5.746835883940462963, 0.7781249993854856273 ) ) ;
#21708 = CARTESIAN_POINT ( 'NONE',  ( -3.756430356249996994, 29.07812499938548356, 8.999999999999992895 ) ) ;
#21709 = EDGE_CURVE ( 'NONE', #5387, #414, #23311, .T. ) ;
#21710 = CARTESIAN_POINT ( 'NONE',  ( 0.000000000000000000, 0.000000000000000000, -6.500000000000000000 ) ) ;
#21711 = DIRECTION ( 'NONE',  ( 0.5877852522924853496, 0.8090169943749385695, 0.000000000000000000 ) ) ;
#21712 = VECTOR ( 'NONE', #7857, 1000.000000000000000 ) ;
#21713 = CARTESIAN_POINT ( 'NONE',  ( -1.999999999999998224, -12.46410161513774639, 0.7500000000000006661 ) ) ;
#21714 = CARTESIAN_POINT ( 'NONE',  ( -1.071796769724494558, -25.93615380933863435, 4.999999999999992895 ) ) ;
#21715 = CARTESIAN_POINT ( 'NONE',  ( 2.000000000000000888, -12.46410161513774817, 2.568749998770967213 ) ) ;
#21716 = CARTESIAN_POINT ( 'NONE',  ( -1.452785157361865531, -31.03863125411923463, -6.500000000000000000 ) ) ;
#21717 = CARTESIAN_POINT ( 'NONE',  ( -4.000000000000003553, -26.29374999877096997, 8.999999999999992895 ) ) ;
#21718 = CARTESIAN_POINT ( 'NONE',  ( -3.756430356249997882, 29.11562499938548143, 11.16877607737301226 ) ) ;
#21719 = CARTESIAN_POINT ( 'NONE',  ( 30.54913349766219710, -5.827558883616158703, 1.000000000000000000 ) ) ;
#21720 = AXIS2_PLACEMENT_3D ( 'NONE', #9669, #19589, #15807 ) ;
#21721 = CYLINDRICAL_SURFACE ( 'NONE', #388, 0.5000000000000000000 ) ;
#21722 = CARTESIAN_POINT ( 'NONE',  ( 3.999999999999996447, -26.06874999877096855, 8.999999999999992895 ) ) ;
#21723 = ORIENTED_EDGE ( 'NONE', *, *, #2128, .F. ) ;
#21724 = DIRECTION ( 'NONE',  ( -0.000000000000000000, -1.000000000000000000, -0.000000000000000000 ) ) ;
#21725 = ORIENTED_EDGE ( 'NONE', *, *, #11499, .T. ) ;
#21726 = AXIS2_PLACEMENT_3D ( 'NONE', #13361, #5890, #13616 ) ;
#21727 = CIRCLE ( 'NONE', #12538, 24.00000000000000355 ) ;
#21728 = ORIENTED_EDGE ( 'NONE', *, *, #19709, .T. ) ;
#21729 = LINE ( 'NONE', #3813, #9964 ) ;
#21730 = ORIENTED_EDGE ( 'NONE', *, *, #19464, .F. ) ;
#21731 = CARTESIAN_POINT ( 'NONE',  ( 3.756430356249995661, -28.59062499938548640, 6.831223922626973533 ) ) ;
#21732 = VERTEX_POINT ( 'NONE', #11540 ) ;
#21733 = LINE ( 'NONE', #14146, #19658 ) ;
#21734 = PRESENTATION_LAYER_ASSIGNMENT (  '', '', ( #15485 ) ) ;
#21735 = VERTEX_POINT ( 'NONE', #17189 ) ;
#21736 = CARTESIAN_POINT ( 'NONE',  ( -1.999999999999995781, 26.95000000000000284, 5.535898384862237620 ) ) ;
#21737 = CARTESIAN_POINT ( 'NONE',  ( 4.000000000000001776, 29.50000000000000711, 8.999999999999992895 ) ) ;
#21738 = AXIS2_PLACEMENT_3D ( 'NONE', #10223, #14036, #9969 ) ;
#21739 = EDGE_CURVE ( 'NONE', #16708, #14667, #15444, .T. ) ;
#21740 = CARTESIAN_POINT ( 'NONE',  ( -30.85476721088022600, 3.897863563850190616, 1.000000000000000000 ) ) ;
#21741 = DIRECTION ( 'NONE',  ( 0.4817536741017267032, 0.8763066800438573667, 0.000000000000000000 ) ) ;
#21742 = CARTESIAN_POINT ( 'NONE',  ( 18.96807563933094798, 21.62427301729024975, 12.25316411605951927 ) ) ;
#21743 = AXIS2_PLACEMENT_3D ( 'NONE', #15032, #24844, #13076 ) ;
#21744 = CARTESIAN_POINT ( 'NONE',  ( 21.21320343559646915, 21.21320343559638744, 8.999999999999992895 ) ) ;
#21745 = AXIS2_PLACEMENT_3D ( 'NONE', #19781, #1878, #9840 ) ;
#21746 = CARTESIAN_POINT ( 'NONE',  ( 3.469446951953614189E-15, 35.50000000000000711, 8.999999999999992895 ) ) ;
#21747 = APPLICATION_PROTOCOL_DEFINITION ( 'draft international standard', 'automotive_design', 1998, #12618 ) ;
#21748 = CARTESIAN_POINT ( 'NONE',  ( 2.000000000000003997, 28.22500000000000142, 5.535898384862238508 ) ) ;
#21749 = ADVANCED_FACE ( 'NONE', ( #5659 ), #21364, .F. ) ;
#21750 = VECTOR ( 'NONE', #2472, 1000.000000000000000 ) ;
#21751 = DIRECTION ( 'NONE',  ( 0.000000000000000000, 0.000000000000000000, 1.000000000000000000 ) ) ;
#21752 = CARTESIAN_POINT ( 'NONE',  ( 19.49840572522085935, 22.15460310318015758, 5.746835883940462963 ) ) ;
#21753 = CARTESIAN_POINT ( 'NONE',  ( -4.000000000000001776, -29.40624999877096357, 11.30940107675849760 ) ) ;
#21754 = VERTEX_POINT ( 'NONE', #1483 ) ;
#21755 = ORIENTED_EDGE ( 'NONE', *, *, #24415, .F. ) ;
#21756 = CARTESIAN_POINT ( 'NONE',  ( -1.878215178124996498, 25.85312499938548925, 5.746835883940462963 ) ) ;
#21757 =( BOUNDED_SURFACE ( )  B_SPLINE_SURFACE ( 1, 2, ( 
 ( #4159, #5866, #21830, #12135, #20112, #9529, #12522, #4300, #16713, #20238, #6631, #22736, #2596, #10558, #18557, #6388, #4815, #638, #20498, #22603, #8606, #22337, #24688, #22213, #14758, #8346, #8726, #4419, #24431, #12790, #6509, #18287, #12393, #2216, #12271, #10173, #16334, #6773, #20360, #14493, #18172, #22460, #375, #2455, #253, #4542, #10418, #16587, #10681, #20636, #18417, #8221, #16194, #24546, #513, #24162, #6253, #14243, #2335, #10295, #24302, #14378, #4686, #8484, #16470, #14623, #12665, #2718, #18670, #756, #17242, #10808, #8996, #21030, #8873, #7292, #889, #20762, #20892, #4932, #13052, #21273, #25212, #7160, #5201, #22857, #13180, #23360, #5449, #3356, #10947, #12915, #9384, #15268, #21150, #19052, #24941, #2841, #2979, #23119, #18801, #22988, #23236, #1409, #3109, #3221, #18938, #7021, #1270, #15151, #16857, #15388, #24822, #6899, #19173, #11193, #1137, #5319, #7408, #15007, #13299 ),
 ( #25074, #11331, #19314, #17363, #25328, #14882, #1022, #9254, #16976, #5073, #11074, #9110, #17099, #25712, #21652, #1655, #9632, #9495, #15772, #19435, #21793, #3876, #5583, #15656, #13441, #3492, #17478, #15908, #11847, #25450, #5700, #17610, #25587, #23741, #7671, #11463, #15530, #3734, #23622, #13679, #7535, #5828, #1526, #19818, #1919, #13564, #11718, #21411, #23496, #21529, #23881, #9880, #3611, #19695, #1794, #9762, #13814, #17741, #11580, #19552, #17866, #7793, #25838, #91, #18002, #7921, #13949, #5966, #21917, #8062, #3998, #11965, #19936, #2040, #10008, #16045, #24007, #6349, #22037, #14462, #18378, #22424, #4505, #2301, #478, #215, #14202, #22175, #2555, #14584, #8447, #12360, #12483, #10138, #6597, #16436, #24400, #24262, #2177, #22304, #724, #14342, #8185, #16163, #10524, #4120, #6476, #18521, #16556, #8575, #20456, #608, #12099, #24515, #10647, #22566, #4647, #24126, #12629, #18141, #6212 ) ),
 .UNSPECIFIED., .F., .F., .F. ) 
 B_SPLINE_SURFACE_WITH_KNOTS ( ( 2, 2 ),
 ( 3, 2, 2, 2, 2, 2, 2, 2, 2, 2, 2, 2, 2, 2, 2, 2, 2, 2, 2, 2, 2, 2, 2, 2, 2, 2, 2, 2, 2, 2, 2, 2, 2, 2, 2, 2, 2, 2, 2, 2, 2, 2, 2, 2, 2, 2, 2, 2, 2, 2, 2, 2, 2, 2, 2, 2, 2, 2, 2, 2, 3 ),
 ( 0.000000000000000000, 1.000000000000000000 ),
 ( 0.000000000000000000, 0.01666666666666666644, 0.03333333333333333287, 0.05000000000000000278, 0.06666666666666666574, 0.08333333333333332871, 0.1000000000000000056, 0.1166666666666666685, 0.1333333333333333315, 0.1499999999999999944, 0.1666666666666666574, 0.1833333333333333204, 0.2000000000000000111, 0.2166666666666666741, 0.2333333333333333370, 0.2500000000000000000, 0.2666666666666666630, 0.2833333333333333259, 0.2999999999999999889, 0.3166666666666666519, 0.3333333333333333148, 0.3499999999999999778, 0.3666666666666666408, 0.3833333333333333592, 0.4000000000000000222, 0.4166666666666666852, 0.4333333333333333481, 0.4500000000000000111, 0.4666666666666666741, 0.4833333333333333370, 0.5000000000000000000, 0.5166666666666667185, 0.5333333333333333259, 0.5500000000000000444, 0.5666666666666666519, 0.5833333333333333703, 0.5999999999999999778, 0.6166666666666666963, 0.6333333333333333037, 0.6500000000000000222, 0.6666666666666666297, 0.6833333333333333481, 0.6999999999999999556, 0.7166666666666666741, 0.7333333333333332815, 0.7500000000000000000, 0.7666666666666667185, 0.7833333333333333259, 0.8000000000000000444, 0.8166666666666666519, 0.8333333333333333703, 0.8499999999999999778, 0.8666666666666666963, 0.8833333333333333037, 0.9000000000000000222, 0.9166666666666666297, 0.9333333333333333481, 0.9499999999999999556, 0.9666666666666666741, 0.9833333333333332815, 1.000000000000000000 ),
 .UNSPECIFIED. ) 
 GEOMETRIC_REPRESENTATION_ITEM ( )  RATIONAL_B_SPLINE_SURFACE ( (
 ( 1.000000000000000000, 0.8660254037844387076, 1.000000000000000000, 0.8660254037844387076, 1.000000000000000000, 0.8660254037844387076, 1.000000000000000000, 0.8660254037844387076, 1.000000000000000000, 0.8660254037844387076, 1.000000000000000000, 0.8660254037844387076, 1.000000000000000000, 0.8660254037844387076, 1.000000000000000000, 0.8660254037844387076, 1.000000000000000000, 0.8660254037844387076, 1.000000000000000000, 0.8660254037844387076, 1.000000000000000000, 0.8660254037844387076, 1.000000000000000000, 0.8660254037844387076, 1.000000000000000000, 0.8660254037844387076, 1.000000000000000000, 0.8660254037844387076, 1.000000000000000000, 0.8660254037844387076, 1.000000000000000000, 0.8660254037844387076, 1.000000000000000000, 0.8660254037844387076, 1.000000000000000000, 0.8660254037844387076, 1.000000000000000000, 0.8660254037844387076, 1.000000000000000000, 0.8660254037844387076, 1.000000000000000000, 0.8660254037844387076, 1.000000000000000000, 0.8660254037844387076, 1.000000000000000000, 0.8660254037844387076, 1.000000000000000000, 0.8660254037844387076, 1.000000000000000000, 0.8660254037844387076, 1.000000000000000000, 0.8660254037844387076, 1.000000000000000000, 0.8660254037844387076, 1.000000000000000000, 0.8660254037844387076, 1.000000000000000000, 0.8660254037844387076, 1.000000000000000000, 0.8660254037844387076, 1.000000000000000000, 0.8660254037844387076, 1.000000000000000000, 0.8660254037844387076, 1.000000000000000000, 0.8660254037844387076, 1.000000000000000000, 0.8660254037844387076, 1.000000000000000000, 0.8660254037844387076, 1.000000000000000000, 0.8660254037844387076, 1.000000000000000000, 0.8660254037844387076, 1.000000000000000000, 0.8660254037844387076, 1.000000000000000000, 0.8660254037844387076, 1.000000000000000000, 0.8660254037844387076, 1.000000000000000000, 0.8660254037844387076, 1.000000000000000000, 0.8660254037844387076, 1.000000000000000000, 0.8660254037844387076, 1.000000000000000000, 0.8660254037844387076, 1.000000000000000000, 0.8660254037844387076, 1.000000000000000000, 0.8660254037844387076, 1.000000000000000000, 0.8660254037844387076, 1.000000000000000000, 0.8660254037844387076, 1.000000000000000000, 0.8660254037844387076, 1.000000000000000000, 0.8660254037844387076, 1.000000000000000000, 0.8660254037844387076, 1.000000000000000000, 0.8660254037844387076, 1.000000000000000000, 0.8660254037844387076, 1.000000000000000000, 0.8660254037844387076, 1.000000000000000000, 0.8660254037844387076, 1.000000000000000000, 0.8660254037844387076, 1.000000000000000000, 0.8660254037844387076, 1.000000000000000000, 0.8660254037844387076, 1.000000000000000000, 0.8660254037844387076, 1.000000000000000000, 0.8660254037844387076, 1.000000000000000000),
 ( 1.000000000000000000, 0.8660254037844387076, 1.000000000000000000, 0.8660254037844387076, 1.000000000000000000, 0.8660254037844387076, 1.000000000000000000, 0.8660254037844387076, 1.000000000000000000, 0.8660254037844387076, 1.000000000000000000, 0.8660254037844387076, 1.000000000000000000, 0.8660254037844387076, 1.000000000000000000, 0.8660254037844387076, 1.000000000000000000, 0.8660254037844387076, 1.000000000000000000, 0.8660254037844387076, 1.000000000000000000, 0.8660254037844387076, 1.000000000000000000, 0.8660254037844387076, 1.000000000000000000, 0.8660254037844387076, 1.000000000000000000, 0.8660254037844387076, 1.000000000000000000, 0.8660254037844387076, 1.000000000000000000, 0.8660254037844387076, 1.000000000000000000, 0.8660254037844387076, 1.000000000000000000, 0.8660254037844387076, 1.000000000000000000, 0.8660254037844387076, 1.000000000000000000, 0.8660254037844387076, 1.000000000000000000, 0.8660254037844387076, 1.000000000000000000, 0.8660254037844387076, 1.000000000000000000, 0.8660254037844387076, 1.000000000000000000, 0.8660254037844387076, 1.000000000000000000, 0.8660254037844387076, 1.000000000000000000, 0.8660254037844387076, 1.000000000000000000, 0.8660254037844387076, 1.000000000000000000, 0.8660254037844387076, 1.000000000000000000, 0.8660254037844387076, 1.000000000000000000, 0.8660254037844387076, 1.000000000000000000, 0.8660254037844387076, 1.000000000000000000, 0.8660254037844387076, 1.000000000000000000, 0.8660254037844387076, 1.000000000000000000, 0.8660254037844387076, 1.000000000000000000, 0.8660254037844387076, 1.000000000000000000, 0.8660254037844387076, 1.000000000000000000, 0.8660254037844387076, 1.000000000000000000, 0.8660254037844387076, 1.000000000000000000, 0.8660254037844387076, 1.000000000000000000, 0.8660254037844387076, 1.000000000000000000, 0.8660254037844387076, 1.000000000000000000, 0.8660254037844387076, 1.000000000000000000, 0.8660254037844387076, 1.000000000000000000, 0.8660254037844387076, 1.000000000000000000, 0.8660254037844387076, 1.000000000000000000, 0.8660254037844387076, 1.000000000000000000, 0.8660254037844387076, 1.000000000000000000, 0.8660254037844387076, 1.000000000000000000, 0.8660254037844387076, 1.000000000000000000, 0.8660254037844387076, 1.000000000000000000, 0.8660254037844387076, 1.000000000000000000, 0.8660254037844387076, 1.000000000000000000, 0.8660254037844387076, 1.000000000000000000, 0.8660254037844387076, 1.000000000000000000, 0.8660254037844387076, 1.000000000000000000, 0.8660254037844387076, 1.000000000000000000, 0.8660254037844387076, 1.000000000000000000, 0.8660254037844387076, 1.000000000000000000, 0.8660254037844387076, 1.000000000000000000, 0.8660254037844387076, 1.000000000000000000) ) ) 
 REPRESENTATION_ITEM ( '' )  SURFACE ( )  );
#21758 = EDGE_LOOP ( 'NONE', ( #20305, #1495, #10458, #6502 ) ) ;
#21759 = CARTESIAN_POINT ( 'NONE',  ( -3.999999999999996447, 26.06874999877096855, 8.999999999999992895 ) ) ;
#21760 = CARTESIAN_POINT ( 'NONE',  ( 21.21320343559646915, 21.21320343559638744, 4.999999999999992006 ) ) ;
#21761 = CARTESIAN_POINT ( 'NONE',  ( 0.000000000000000000, 0.000000000000000000, -6.500000000000000000 ) ) ;
#21762 = ORIENTED_EDGE ( 'NONE', *, *, #925, .F. ) ;
#21763 = ORIENTED_EDGE ( 'NONE', *, *, #16940, .T. ) ;
#21764 = AXIS2_PLACEMENT_3D ( 'NONE', #6616, #18542, #22446 ) ;
#21765 = FACE_OUTER_BOUND ( 'NONE', #22074, .T. ) ;
#21766 = ORIENTED_EDGE ( 'NONE', *, *, #12325, .F. ) ;
#21767 = CARTESIAN_POINT ( 'NONE',  ( -0.7500000000000001110, 0.000000000000000000, 17.69999999999999929 ) ) ;
#21768 = CARTESIAN_POINT ( 'NONE',  ( -1.499999999999998224, -7.499999999999992895, 25.00000000000000000 ) ) ;
#21769 = CARTESIAN_POINT ( 'NONE',  ( 1.878215178125005158, 28.81562499938548783, 5.746835883940462963 ) ) ;
#21770 = AXIS2_PLACEMENT_3D ( 'NONE', #12900, #8591, #20747 ) ;
#21771 = FACE_OUTER_BOUND ( 'NONE', #1311, .T. ) ;
#21772 = CARTESIAN_POINT ( 'NONE',  ( 2.000000000000000000, 26.27500000000000568, 12.46410161513774817 ) ) ;
#21773 = EDGE_CURVE ( 'NONE', #7744, #15159, #15855, .T. ) ;
#21774 = DIRECTION ( 'NONE',  ( -0.000000000000000000, -1.000000000000000000, -0.000000000000000000 ) ) ;
#21775 = EDGE_CURVE ( 'NONE', #246, #161, #4135, .T. ) ;
#21776 =( NAMED_UNIT ( * ) SI_UNIT ( $, .STERADIAN. ) SOLID_ANGLE_UNIT ( ) );
#21777 = AXIS2_PLACEMENT_3D ( 'NONE', #4251, #327, #22167 ) ;
#21778 = AXIS2_PLACEMENT_3D ( 'NONE', #6440, #8406, #14814 ) ;
#21779 = CARTESIAN_POINT ( 'NONE',  ( -1.999999999999998224, -12.46410161513774639, 1.143749998770968279 ) ) ;
#21780 = CARTESIAN_POINT ( 'NONE',  ( 0.000000000000000000, 0.000000000000000000, 1.000000000000000000 ) ) ;
#21781 = CARTESIAN_POINT ( 'NONE',  ( 19.99344423804966198, 17.16501711330340996, 12.46410161513774817 ) ) ;
#21782 = AXIS2_PLACEMENT_3D ( 'NONE', #1385, #25692, #19286 ) ;
#21783 = CARTESIAN_POINT ( 'NONE',  ( 16.92403133439988139, 22.23642609031855244, 6.831223922626973533 ) ) ;
#21784 = EDGE_CURVE ( 'NONE', #17935, #20933, #11146, .T. ) ;
#21785 = CARTESIAN_POINT ( 'NONE',  ( 4.000000000000049738, -6.690598923241514839, 4.481249998770968190 ) ) ;
#21786 = CARTESIAN_POINT ( 'NONE',  ( 1.071796769724498999, 28.05759618943233491, 12.99999999999998757 ) ) ;
#21787 = AXIS2_PLACEMENT_3D ( 'NONE', #14842, #20591, #8297 ) ;
#21788 = DIRECTION ( 'NONE',  ( 0.000000000000000000, 0.000000000000000000, 1.000000000000000000 ) ) ;
#21789 = PLANE ( 'NONE',  #22539 ) ;
#21790 = DIRECTION ( 'NONE',  ( 0.000000000000000000, 0.000000000000000000, 1.000000000000000000 ) ) ;
#21791 = ORIENTED_EDGE ( 'NONE', *, *, #620, .T. ) ;
#21792 = CARTESIAN_POINT ( 'NONE',  ( -1.999999999999995781, 26.89374999877097139, 5.535898384862237620 ) ) ;
#21793 = CARTESIAN_POINT ( 'NONE',  ( 1.999999999999998224, -25.75000000000000355, 12.46410161513774639 ) ) ;
#21795 = VERTEX_POINT ( 'NONE', #15222 ) ;
#21794 = DIRECTION ( 'NONE',  ( -0.000000000000000000, 1.000000000000000000, -0.000000000000000000 ) ) ;
#21796 = CARTESIAN_POINT ( 'NONE',  ( 3.735045420075836212E-15, 28.51562499938548356, 4.662447845253954171 ) ) ;
#21798 = FACE_OUTER_BOUND ( 'NONE', #22135, .T. ) ;
#21797 = AXIS2_PLACEMENT_3D ( 'NONE', #21656, #23501, #11969 ) ;
#21799 = VERTEX_POINT ( 'NONE', #1361 ) ;
#21800 = DIRECTION ( 'NONE',  ( -0.000000000000000000, 0.000000000000000000, 1.000000000000000000 ) ) ;
#21801 = ORIENTED_EDGE ( 'NONE', *, *, #20668, .F. ) ;
#21802 = EDGE_LOOP ( 'NONE', ( #17144, #287, #12851, #23779 ) ) ;
#21803 = CARTESIAN_POINT ( 'NONE',  ( -10.98232076577242644, -29.09636799667071116, -2.750000000000000000 ) ) ;
#21804 = CARTESIAN_POINT ( 'NONE',  ( -1.878215178124996498, 29.45312499938548711, 5.746835883940462963 ) ) ;
#21805 = AXIS2_PLACEMENT_3D ( 'NONE', #17541, #151, #17921 ) ;
#21806 = CARTESIAN_POINT ( 'NONE',  ( 3.756430356250003655, -8.999999999999992895, 2.840624999385484184 ) ) ;
#21807 = VECTOR ( 'NONE', #21630, 1000.000000000000000 ) ;
#21808 = AXIS2_PLACEMENT_3D ( 'NONE', #22202, #12261, #3902 ) ;
#21809 = CARTESIAN_POINT ( 'NONE',  ( 19.14933551713917126, 19.14933551713910376, 12.99999999999999289 ) ) ;
#21810 = LINE ( 'NONE', #17881, #23478 ) ;
#21811 = CARTESIAN_POINT ( 'NONE',  ( 17.83234913717923220, 23.48920338667153729, 8.999999999999992895 ) ) ;
#21812 = AXIS2_PLACEMENT_3D ( 'NONE', #675, #10852, #22372 ) ;
#21813 = CARTESIAN_POINT ( 'NONE',  ( 1.999999999999998224, 29.36874999877097636, 12.46410161513774817 ) ) ;
#21814 = CARTESIAN_POINT ( 'NONE',  ( -24.86329371854747805, 18.68225429291759099, -6.500000000000000000 ) ) ;
#21815 = CARTESIAN_POINT ( 'NONE',  ( 5.112995299272250684E-15, 26.40624999877096712, 4.999999999999992006 ) ) ;
#21816 = CARTESIAN_POINT ( 'NONE',  ( 0.000000000000000000, 10.00000000000000000, 15.00000000000000178 ) ) ;
#21817 = DIRECTION ( 'NONE',  ( 1.000000000000000000, 0.000000000000000000, 0.000000000000000000 ) ) ;
#21818 = EDGE_CURVE ( 'NONE', #1926, #2494, #17516, .T. ) ;
#21819 = ORIENTED_EDGE ( 'NONE', *, *, #19234, .T. ) ;
#21820 = CARTESIAN_POINT ( 'NONE',  ( -3.369928719974892281E-15, -25.11250000000000426, 4.999999999999992006 ) ) ;
#21821 = LINE ( 'NONE', #24152, #24667 ) ;
#21822 = CARTESIAN_POINT ( 'NONE',  ( -1.878215178124998497, 26.90312499938548285, 12.25316411605951927 ) ) ;
#21823 = EDGE_CURVE ( 'NONE', #17660, #8728, #5537, .T. ) ;
#21824 = AXIS2_PLACEMENT_3D ( 'NONE', #14689, #2905, #24118 ) ;
#21825 = CYLINDRICAL_SURFACE ( 'NONE', #14969, 0.5000000000000004441 ) ;
#21826 = CARTESIAN_POINT ( 'NONE',  ( -4.000000000000000888, 29.25624999877096855, 11.30940107675849404 ) ) ;
#21827 = DIRECTION ( 'NONE',  ( 0.000000000000000000, 0.000000000000000000, 1.000000000000000000 ) ) ;
#21828 = ORIENTED_EDGE ( 'NONE', *, *, #19003, .F. ) ;
#21829 = CARTESIAN_POINT ( 'NONE',  ( 4.000000000000003553, -8.999999999999992895, 2.700000000000001066 ) ) ;
#21830 = CARTESIAN_POINT ( 'NONE',  ( -1.878215178125004048, -25.21562499938548285, 5.746835883940462963 ) ) ;
#21831 = VERTEX_POINT ( 'NONE', #1606 ) ;
#21832 = ORIENTED_EDGE ( 'NONE', *, *, #24343, .F. ) ;
#21833 = ORIENTED_EDGE ( 'NONE', *, *, #25853, .F. ) ;
#21834 = VERTEX_POINT ( 'NONE', #37 ) ;
#21835 = ORIENTED_EDGE ( 'NONE', *, *, #8635, .T. ) ;
#21836 = CARTESIAN_POINT ( 'NONE',  ( -27.10000000000000497, 0.6000000000000000888, 19.59999999999999787 ) ) ;
#21837 = CARTESIAN_POINT ( 'NONE',  ( -3.028776527127584828, 38.71721868403346178, 13.92618862263473289 ) ) ;
#21838 = CIRCLE ( 'NONE', #958, 0.5000000000000004441 ) ;
#21839 = CARTESIAN_POINT ( 'NONE',  ( -1.878215178124999829, 27.69062499938549138, 12.25316411605951927 ) ) ;
#21840 = VECTOR ( 'NONE', #7194, 1000.000000000000000 ) ;
#21841 = CARTESIAN_POINT ( 'NONE',  ( -1.878215178124995832, -5.746835883940462963, 3.890624999385482674 ) ) ;
#21842 = CARTESIAN_POINT ( 'NONE',  ( 2.620986760973688460E-15, -13.61880215351699874, 3.431249998770965703 ) ) ;
#21843 = CARTESIAN_POINT ( 'NONE',  ( -1.878215178124995832, 29.45312499938548356, 5.746835883940462963 ) ) ;
#21844 = CARTESIAN_POINT ( 'NONE',  ( 3.878215178125003604, 25.07031249969274356, 8.999999999999992895 ) ) ;
#21845 = DIRECTION ( 'NONE',  ( -0.8660254037844397068, 0.4999999999999983347, -0.000000000000000000 ) ) ;
#21846 = CIRCLE ( 'NONE', #25193, 31.10000000000000142 ) ;
#21847 = ADVANCED_FACE ( 'NONE', ( #2259 ), #13903, .T. ) ;
#21848 = CARTESIAN_POINT ( 'NONE',  ( 4.000000000000003553, -6.690598923241489970, 1.837499999999995914 ) ) ;
#21849 = CARTESIAN_POINT ( 'NONE',  ( -3.999999999999996447, -8.999999999999992895, 1.125000000000000888 ) ) ;
#21850 = CARTESIAN_POINT ( 'NONE',  ( -4.000000000000002665, -29.87009603951200276, 10.45670610619353980 ) ) ;
#21851 = CARTESIAN_POINT ( 'NONE',  ( 0.000000000000000000, 0.000000000000000000, -6.500000000000000000 ) ) ;
#21852 = CARTESIAN_POINT ( 'NONE',  ( -2.000000000000003997, -28.61874999877096926, 5.535898384862238508 ) ) ;
#21853 = CARTESIAN_POINT ( 'NONE',  ( 1.878215178125004048, 27.57812499938548711, 5.746835883940462963 ) ) ;
#21854 = EDGE_CURVE ( 'NONE', #24465, #5387, #1639, .T. ) ;
#21855 = FACE_OUTER_BOUND ( 'NONE', #4820, .T. ) ;
#21856 = AXIS2_PLACEMENT_3D ( 'NONE', #13026, #3851, #5943 ) ;
#21857 = DIRECTION ( 'NONE',  ( 0.000000000000000000, 0.000000000000000000, 1.000000000000000000 ) ) ;
#21858 = CARTESIAN_POINT ( 'NONE',  ( 3.999999999999997335, -26.10624999877096997, 11.30940107675849404 ) ) ;
#21859 = VERTEX_POINT ( 'NONE', #14153 ) ;
#21860 = CARTESIAN_POINT ( 'NONE',  ( -1.071796769724487675, -29.14240381056766438, 4.999999999999988454 ) ) ;
#21862 = ORIENTED_EDGE ( 'NONE', *, *, #19056, .F. ) ;
#21861 = CARTESIAN_POINT ( 'NONE',  ( -3.735045420075836212E-15, -28.85312499938548569, 4.662447845253954171 ) ) ;
#21863 = ORIENTED_EDGE ( 'NONE', *, *, #21291, .F. ) ;
#21864 = FACE_OUTER_BOUND ( 'NONE', #12030, .T. ) ;
#21865 = VERTEX_POINT ( 'NONE', #22121 ) ;
#21866 = CARTESIAN_POINT ( 'NONE',  ( 1.878215178124998497, -26.34062499938548285, 12.25316411605951927 ) ) ;
#21867 = ORIENTED_EDGE ( 'NONE', *, *, #25431, .T. ) ;
#21868 = CARTESIAN_POINT ( 'NONE',  ( 21.37230246136343581, 18.54387533661716958, 5.535898384862238508 ) ) ;
#21869 = EDGE_CURVE ( 'NONE', #18350, #8164, #22945, .T. ) ;
#21870 = ORIENTED_EDGE ( 'NONE', *, *, #17842, .T. ) ;
#21871 = CARTESIAN_POINT ( 'NONE',  ( 4.000000000000003553, 28.63750000000000284, 6.690598923241489970 ) ) ;
#21872 = CARTESIAN_POINT ( 'NONE',  ( 2.672651547586948120E-15, 26.94062499938548783, 13.33755215474603162 ) ) ;
#21873 = AXIS2_PLACEMENT_3D ( 'NONE', #8111, #17908, #3534 ) ;
#21874 = CARTESIAN_POINT ( 'NONE',  ( -3.756430356249996994, -8.999999999999992895, 0.9281249993854829849 ) ) ;
#21875 = DIRECTION ( 'NONE',  ( 0.000000000000000000, 0.000000000000000000, -1.000000000000000000 ) ) ;
#21876 = CARTESIAN_POINT ( 'NONE',  ( 18.54381157061901675, 21.20000894857831852, 5.746835883940462963 ) ) ;
#21877 = CARTESIAN_POINT ( 'NONE',  ( 3.469446951953614189E-15, 40.00000000000000000, 8.999999999999992895 ) ) ;
#21878 = DIRECTION ( 'NONE',  ( 0.000000000000000000, 0.000000000000000000, -1.000000000000000000 ) ) ;
#21879 = CARTESIAN_POINT ( 'NONE',  ( -3.999999999999997335, 29.31250000000000000, 11.30940107675849404 ) ) ;
#21880 = CARTESIAN_POINT ( 'NONE',  ( -3.756430356249997438, -11.16877607737301048, 0.5156249993854836733 ) ) ;
#21881 = CARTESIAN_POINT ( 'NONE',  ( 22.71372316761954480, 17.40132841170072453, 11.16877607737301403 ) ) ;
#21882 = FACE_OUTER_BOUND ( 'NONE', #510, .T. ) ;
#21883 = PRESENTATION_LAYER_ASSIGNMENT (  '', '', ( #3510 ) ) ;
#21884 = ORIENTED_EDGE ( 'NONE', *, *, #19062, .F. ) ;
#21885 = ORIENTED_EDGE ( 'NONE', *, *, #23851, .F. ) ;
#21886 = CARTESIAN_POINT ( 'NONE',  ( 6.009258394948636914E-15, 29.10624999877097352, 4.381197846482986158 ) ) ;
#21887 = ADVANCED_FACE ( 'NONE', ( #172 ), #23828, .F. ) ;
#21888 = ORIENTED_EDGE ( 'NONE', *, *, #10589, .F. ) ;
#21889 = DIRECTION ( 'NONE',  ( 0.000000000000000000, 0.000000000000000000, -1.000000000000000000 ) ) ;
#21890 = CARTESIAN_POINT ( 'NONE',  ( 2.000000000000000888, 29.36874999877096926, 12.46410161513774817 ) ) ;
#21891 = CARTESIAN_POINT ( 'NONE',  ( 3.756430356250002323, 29.71562499938548640, 11.16877607737301226 ) ) ;
#21892 = CARTESIAN_POINT ( 'NONE',  ( 1.071796769724494558, 28.18615380933863435, 4.999999999999992895 ) ) ;
#21893 = ORIENTED_EDGE ( 'NONE', *, *, #22936, .F. ) ;
#21894 = EDGE_CURVE ( 'NONE', #6294, #7204, #3718, .T. ) ;
#21895 = CARTESIAN_POINT ( 'NONE',  ( -4.000000000000000000, 26.06874999877097210, 8.999999999999992895 ) ) ;
#21896 = EDGE_LOOP ( 'NONE', ( #3837, #16649, #443, #20204 ) ) ;
#21897 = CARTESIAN_POINT ( 'NONE',  ( 3.526711513754840599, 38.89679573513954125, 4.645898033750303746 ) ) ;
#21898 = CARTESIAN_POINT ( 'NONE',  ( 1.878215178125000939, 27.76562499938548356, 12.25316411605952283 ) ) ;
#21899 = CARTESIAN_POINT ( 'NONE',  ( -1.878215178124998275, 27.24062499938548854, 12.25316411605951927 ) ) ;
#21900 = VECTOR ( 'NONE', #21889, 1000.000000000000000 ) ;
#21901 = CARTESIAN_POINT ( 'NONE',  ( 0.3338636427494953152, 38.86740601410824070, 3.377184973053767969 ) ) ;
#21902 = CARTESIAN_POINT ( 'NONE',  ( 0.000000000000000000, 0.000000000000000000, -6.500000000000000000 ) ) ;
#21903 = CARTESIAN_POINT ( 'NONE',  ( 4.000000000000005329, 28.18750000000000711, 6.690598923241489970 ) ) ;
#21904 = CARTESIAN_POINT ( 'NONE',  ( 3.756430356250004099, 26.52812499938548285, 6.831223922626973533 ) ) ;
#21905 = DIRECTION ( 'NONE',  ( 0.000000000000000000, 0.000000000000000000, 1.000000000000000000 ) ) ;
#21906 = CIRCLE ( 'NONE', #7303, 31.10000000000000142 ) ;
#21907 = DIRECTION ( 'NONE',  ( 0.000000000000000000, 1.000000000000000000, 0.000000000000000000 ) ) ;
#21908 = CARTESIAN_POINT ( 'NONE',  ( 19.98460540328484214, 19.98460540328476398, 4.381197846482986158 ) ) ;
#21909 = FACE_OUTER_BOUND ( 'NONE', #18410, .T. ) ;
#21910 = CARTESIAN_POINT ( 'NONE',  ( 0.000000000000000000, 10.00000000000000000, 17.00000000000000000 ) ) ;
#21911 = CARTESIAN_POINT ( 'NONE',  ( -1.878215178124998497, 29.04062499938548569, 12.25316411605951927 ) ) ;
#21912 = CYLINDRICAL_SURFACE ( 'NONE', #13733, 0.5000000000000004441 ) ;
#21913 = EDGE_CURVE ( 'NONE', #24200, #2002, #19184, .T. ) ;
#21914 = CARTESIAN_POINT ( 'NONE',  ( 19.20672417798141041, 21.86292155594071218, 12.25316411605951927 ) ) ;
#21915 = ORIENTED_EDGE ( 'NONE', *, *, #18631, .F. ) ;
#21916 = CARTESIAN_POINT ( 'NONE',  ( -3.999999999999996447, 26.51874999877097139, 8.999999999999992895 ) ) ;
#21917 = CARTESIAN_POINT ( 'NONE',  ( 1.999999999999998224, -27.55000000000000071, 12.46410161513774639 ) ) ;
#21919 = ORIENTED_EDGE ( 'NONE', *, *, #4132, .T. ) ;
#21918 = CARTESIAN_POINT ( 'NONE',  ( 1.878215178125001605, 27.87812499938548783, 12.25316411605952283 ) ) ;
#21920 = CARTESIAN_POINT ( 'NONE',  ( 3.756430356250002323, 27.91562499938548569, 11.16877607737301403 ) ) ;
#21921 = EDGE_CURVE ( 'NONE', #1666, #20500, #16120, .T. ) ;
#21922 = DIRECTION ( 'NONE',  ( 0.7705132427757873659, -0.6374239897486919659, 0.000000000000000000 ) ) ;
#21923 = CARTESIAN_POINT ( 'NONE',  ( 0.4999838450259764255, 31.09598070739550124, -6.500000000000000000 ) ) ;
#21924 = DIRECTION ( 'NONE',  ( -0.000000000000000000, -0.000000000000000000, 1.000000000000000000 ) ) ;
#21925 = ORIENTED_EDGE ( 'NONE', *, *, #204, .T. ) ;
#21926 = VERTEX_POINT ( 'NONE', #25785 ) ;
#21927 = EDGE_CURVE ( 'NONE', #9386, #13117, #13759, .T. ) ;
#21928 = CARTESIAN_POINT ( 'NONE',  ( -3.756430356250003655, -25.25312499938548427, 8.999999999999992895 ) ) ;
#21929 = CARTESIAN_POINT ( 'NONE',  ( -1.878215178124996498, 25.74062499938548854, 5.746835883940462963 ) ) ;
#21930 = CARTESIAN_POINT ( 'NONE',  ( -3.756430356249996105, -6.831223922626973533, 4.378124999385480720 ) ) ;
#21931 = EDGE_CURVE ( 'NONE', #2220, #5530, #23780, .T. ) ;
#21932 = AXIS2_PLACEMENT_3D ( 'NONE', #6280, #18693, #18192 ) ;
#21933 = DIRECTION ( 'NONE',  ( 0.000000000000000000, 0.000000000000000000, 1.000000000000000000 ) ) ;
#21934 =( LENGTH_UNIT ( ) NAMED_UNIT ( * ) SI_UNIT ( .MILLI., .METRE. ) );
#21935 = LINE ( 'NONE', #20092, #22227 ) ;
#21936 = DIRECTION ( 'NONE',  ( -0.000000000000000000, -0.000000000000000000, -1.000000000000000000 ) ) ;
#21937 = CARTESIAN_POINT ( 'NONE',  ( 19.35704813498177046, 16.52862101023551844, 12.46410161513774817 ) ) ;
#21938 = LINE ( 'NONE', #2201, #18330 ) ;
#21940 = EDGE_CURVE ( 'NONE', #16864, #18179, #7870, .T. ) ;
#21939 = CARTESIAN_POINT ( 'NONE',  ( 2.620986760973688460E-15, -13.61880215351699874, 2.081249998770966947 ) ) ;
#21941 = CARTESIAN_POINT ( 'NONE',  ( 15.89664432368105551, 21.55349857317336415, 6.690598923241487306 ) ) ;
#21942 = ORIENTED_EDGE ( 'NONE', *, *, #21931, .F. ) ;
#21943 = DIRECTION ( 'NONE',  ( 0.000000000000000000, 1.000000000000000000, 0.000000000000000000 ) ) ;
#21944 = CARTESIAN_POINT ( 'NONE',  ( 5.706339097771728319, 38.63519838069890966, 7.645898033751371337 ) ) ;
#21945 = CARTESIAN_POINT ( 'NONE',  ( -1.878215178124995832, 28.10312499938548569, 5.746835883940462963 ) ) ;
#21946 = DIRECTION ( 'NONE',  ( 0.000000000000000000, 0.000000000000000000, 1.000000000000000000 ) ) ;
#21947 = CARTESIAN_POINT ( 'NONE',  ( 8.831537335106614961E-15, 26.63124999877096855, 12.99999999999999112 ) ) ;
#21948 = CARTESIAN_POINT ( 'NONE',  ( -29.99470236596021167, 8.217531866531519569, -6.500000000000000000 ) ) ;
#21949 = EDGE_LOOP ( 'NONE', ( #10899, #23238, #21064, #16923 ) ) ;
#21950 = DIRECTION ( 'NONE',  ( 1.000000000000000000, 0.000000000000000000, 0.000000000000000000 ) ) ;
#21951 = CARTESIAN_POINT ( 'NONE',  ( 3.756430356250003655, 29.64062499938548356, 8.999999999999992895 ) ) ;
#21953 = VERTEX_POINT ( 'NONE', #20159 ) ;
#21952 = DIRECTION ( 'NONE',  ( -0.000000000000000000, -0.000000000000000000, -1.000000000000000000 ) ) ;
#21954 = VERTEX_POINT ( 'NONE', #18213 ) ;
#21955 = VERTEX_POINT ( 'NONE', #14295 ) ;
#21956 = VECTOR ( 'NONE', #798, 1000.000000000000000 ) ;
#21957 = ORIENTED_EDGE ( 'NONE', *, *, #12069, .T. ) ;
#21958 = EDGE_CURVE ( 'NONE', #961, #9527, #3825, .T. ) ;
#21959 = DIRECTION ( 'NONE',  ( 0.000000000000000000, 0.000000000000000000, 1.000000000000000000 ) ) ;
#21960 = CARTESIAN_POINT ( 'NONE',  ( 3.469446951953614189E-15, 40.00000000000000000, 8.999999999999992895 ) ) ;
#21961 = SURFACE_SIDE_STYLE ('',( #3788 ) ) ;
#21962 = EDGE_CURVE ( 'NONE', #7351, #20735, #7914, .T. ) ;
#21963 = CARTESIAN_POINT ( 'NONE',  ( -3.756430356249996105, 26.67812499938548854, 6.831223922626973533 ) ) ;
#21964 = EDGE_CURVE ( 'NONE', #5871, #17035, #5400, .T. ) ;
#21965 = CIRCLE ( 'NONE', #3576, 0.5000000000000003331 ) ;
#21966 = CARTESIAN_POINT ( 'NONE',  ( -3.756430356249996994, -8.999999999999992895, 1.715624999385483074 ) ) ;
#21967 = CARTESIAN_POINT ( 'NONE',  ( 4.000000000000003553, -6.690598923241489970, 3.131249998770965881 ) ) ;
#21968 = CARTESIAN_POINT ( 'NONE',  ( 2.672651547586948120E-15, 28.74062499938548498, 13.33755215474602984 ) ) ;
#21969 = DIRECTION ( 'NONE',  ( 0.000000000000000000, 0.000000000000000000, 1.000000000000000000 ) ) ;
#21970 = B_SPLINE_CURVE_WITH_KNOTS ( 'NONE', 3,
 ( #23663, #13487, #5741, #21837, #6009, #13990, #21454, #4040, #3533, #11505, #13720, #21699, #3786, #20368, #20646, #18430 ),
 .UNSPECIFIED., .F., .F.,
 ( 4, 2, 2, 2, 2, 2, 2, 4 ),
 ( 2.789812635117653453E-07, 0.0002322844908107169664, 0.0004642900003579222032, 0.0006962955099051274400, 0.0009283010194523326226, 0.001160306528999537805, 0.001392312038546742988, 0.001856323057641153353 ),
 .UNSPECIFIED. ) ;
#21971 = CARTESIAN_POINT ( 'NONE',  ( -25.16042852506064165, 18.28012134629622309, 1.000000000000000000 ) ) ;
#21972 = CARTESIAN_POINT ( 'NONE',  ( -3.756430356249996105, 27.12812499938548427, 6.831223922626973533 ) ) ;
#21973 = APPLICATION_CONTEXT ( 'automotive_design' ) ;
#21974 = CYLINDRICAL_SURFACE ( 'NONE', #6691, 4.000000000000000000 ) ;
#21975 = DIRECTION ( 'NONE',  ( 0.000000000000000000, 0.000000000000000000, 1.000000000000000000 ) ) ;
#21976 = CARTESIAN_POINT ( 'NONE',  ( 3.999999999999997335, -29.25624999877096499, 11.30940107675849404 ) ) ;
#21977 = CARTESIAN_POINT ( 'NONE',  ( 2.672651547586948120E-15, 28.29062499938548569, 13.33755215474602984 ) ) ;
#21978 = DIRECTION ( 'NONE',  ( 1.000000000000000000, 0.000000000000000000, 0.000000000000000000 ) ) ;
#21979 = CARTESIAN_POINT ( 'NONE',  ( -1.057460391440397258E-14, 29.55624999877096926, 4.999999999999992006 ) ) ;
#21980 = LINE ( 'NONE', #12165, #23500 ) ;
#21981 = EDGE_LOOP ( 'NONE', ( #519, #24342, #164, #24044 ) ) ;
#21982 = CARTESIAN_POINT ( 'NONE',  ( 4.000000000000003553, 28.60000000000000142, 8.999999999999992895 ) ) ;
#21984 = ORIENTED_EDGE ( 'NONE', *, *, #17042, .T. ) ;
#21983 = DIRECTION ( 'NONE',  ( 0.000000000000000000, 0.000000000000000000, 1.000000000000000000 ) ) ;
#21985 =( BOUNDED_CURVE ( )  B_SPLINE_CURVE ( 2, ( #23399, #19590, #3643, #4032, #9795, #5733, #13984, #1950, #1695 ),
 .UNSPECIFIED., .F., .F. ) 
 B_SPLINE_CURVE_WITH_KNOTS ( ( 3, 2, 2, 2, 3 ),
 ( 0.6750000000000000444, 0.6833333333333333481, 0.6999999999999999556, 0.7166666666666666741, 0.7249999999999999778 ),
 .UNSPECIFIED. ) 
 CURVE ( )  GEOMETRIC_REPRESENTATION_ITEM ( )  RATIONAL_B_SPLINE_CURVE ( ( 0.9330127018922194093, 0.9330127018922198534, 1.000000000000000000, 0.8660254037844387076, 1.000000000000000000, 0.8660254037844387076, 1.000000000000000000, 0.9330127018922194093, 0.9330127018922194093 ) ) 
 REPRESENTATION_ITEM ( '' )  );
#21986 = ORIENTED_EDGE ( 'NONE', *, *, #15295, .F. ) ;
#21987 = CARTESIAN_POINT ( 'NONE',  ( 0.000000000000000000, 29.78124999877097423, 12.99999999999999289 ) ) ;
#21988 = ORIENTED_EDGE ( 'NONE', *, *, #19522, .F. ) ;
#21989 = ORIENTED_EDGE ( 'NONE', *, *, #21921, .F. ) ;
#21990 = ORIENTED_EDGE ( 'NONE', *, *, #6865, .F. ) ;
#21991 = ORIENTED_EDGE ( 'NONE', *, *, #8746, .T. ) ;
#21992 = DIRECTION ( 'NONE',  ( 0.000000000000000000, 0.000000000000000000, 1.000000000000000000 ) ) ;
#21993 = CARTESIAN_POINT ( 'NONE',  ( 1.878215178125000939, 27.42812499938548498, 12.25316411605952283 ) ) ;
#21994 = EDGE_CURVE ( 'NONE', #19514, #18149, #17131, .T. ) ;
#21995 = DIRECTION ( 'NONE',  ( -0.000000000000000000, -0.000000000000000000, -1.000000000000000000 ) ) ;
#21996 = DIRECTION ( 'NONE',  ( 1.000000000000000000, 0.000000000000000000, 0.000000000000000000 ) ) ;
#21997 = CARTESIAN_POINT ( 'NONE',  ( 15.59820611967510295, 20.91060087559377934, 8.999999999999992895 ) ) ;
#21998 = EDGE_CURVE ( 'NONE', #24266, #9446, #22653, .T. ) ;
#21999 = DIRECTION ( 'NONE',  ( 0.000000000000000000, 1.000000000000000000, 0.000000000000000000 ) ) ;
#22000 = CARTESIAN_POINT ( 'NONE',  ( -30.35476721088022600, 3.897863563850190616, 1.000000000000000000 ) ) ;
#22001 = CARTESIAN_POINT ( 'NONE',  ( -3.999999999999996003, 28.78750000000000142, 6.690598923241487306 ) ) ;
#22002 = CARTESIAN_POINT ( 'NONE',  ( 4.000000000000001776, 29.01249999999999929, 11.30940107675849760 ) ) ;
#22003 = DIRECTION ( 'NONE',  ( -0.000000000000000000, -0.000000000000000000, -1.000000000000000000 ) ) ;
#22004 = CARTESIAN_POINT ( 'NONE',  ( 0.000000000000000000, 0.000000000000000000, 19.50000000000000000 ) ) ;
#22005 = CARTESIAN_POINT ( 'NONE',  ( -22.67092431280609688, -21.28941499438201745, 1.000000000000000000 ) ) ;
#22006 = ORIENTED_EDGE ( 'NONE', *, *, #21515, .F. ) ;
#22007 = ORIENTED_EDGE ( 'NONE', *, *, #13804, .T. ) ;
#22008 = CARTESIAN_POINT ( 'NONE',  ( 1.878215178125001605, 26.52812499938548640, 12.25316411605952283 ) ) ;
#22009 = EDGE_LOOP ( 'NONE', ( #14409, #19320, #1411, #5523 ) ) ;
#22010 = CARTESIAN_POINT ( 'NONE',  ( 8.831537335106614961E-15, 26.23749999999999716, 12.99999999999999112 ) ) ;
#22011 = CARTESIAN_POINT ( 'NONE',  ( -3.756430356249997882, 25.96562499938548640, 11.16877607737301226 ) ) ;
#22012 = CARTESIAN_POINT ( 'NONE',  ( 0.000000000000000000, 0.000000000000000000, -6.500000000000000000 ) ) ;
#22013 = CARTESIAN_POINT ( 'NONE',  ( -1.999999999999998224, 27.49374999877096926, 12.46410161513774639 ) ) ;
#22014 = ORIENTED_EDGE ( 'NONE', *, *, #10821, .F. ) ;
#22015 = CARTESIAN_POINT ( 'NONE',  ( 1.071796769724488563, -25.76740381056766793, 12.99999999999999289 ) ) ;
#22016 = VERTEX_POINT ( 'NONE', #22780 ) ;
#22017 = DIRECTION ( 'NONE',  ( 0.000000000000000000, 0.000000000000000000, 1.000000000000000000 ) ) ;
#22018 = ADVANCED_FACE ( 'NONE', ( #4857 ), #8924, .T. ) ;
#22019 = CARTESIAN_POINT ( 'NONE',  ( 3.756430356250004099, 27.87812499938548427, 6.831223922626973533 ) ) ;
#22020 = CARTESIAN_POINT ( 'NONE',  ( -2.451530025009351910, -31.00322564728512020, -6.500000000000000000 ) ) ;
#22021 = EDGE_CURVE ( 'NONE', #2564, #24580, #16718, .T. ) ;
#22022 = DIRECTION ( 'NONE',  ( -0.000000000000000000, -0.000000000000000000, -1.000000000000000000 ) ) ;
#22023 = CARTESIAN_POINT ( 'NONE',  ( 16.74068927859332234, 19.39688665655263122, 12.25316411605951927 ) ) ;
#22024 = CARTESIAN_POINT ( 'NONE',  ( -3.756430356249996994, 25.81562499938548427, 8.999999999999992895 ) ) ;
#22025 =( NAMED_UNIT ( * ) PLANE_ANGLE_UNIT ( ) SI_UNIT ( $, .RADIAN. ) );
#22026 = EDGE_CURVE ( 'NONE', #1168, #12794, #18596, .T. ) ;
#22027 = DIRECTION ( 'NONE',  ( 0.000000000000000000, 0.000000000000000000, 1.000000000000000000 ) ) ;
#22028 = DIRECTION ( 'NONE',  ( 0.000000000000000000, 0.000000000000000000, 1.000000000000000000 ) ) ;
#22029 = CARTESIAN_POINT ( 'NONE',  ( 17.11198410471449094, 19.94041122946061151, 12.46410161513774639 ) ) ;
#22030 = CARTESIAN_POINT ( 'NONE',  ( 3.469446951953614189E-15, -8.999999999999992895, -10.00000000000000000 ) ) ;
#22031 = DIRECTION ( 'NONE',  ( 0.4257792915650852050, 0.9048270524660135816, 0.000000000000000000 ) ) ;
#22032 = CARTESIAN_POINT ( 'NONE',  ( 23.03842281366517852, 17.38156856417272422, 6.690598923241489970 ) ) ;
#22033 = AXIS2_PLACEMENT_3D ( 'NONE', #18897, #19266, #1369 ) ;
#22034 = CARTESIAN_POINT ( 'NONE',  ( 18.17030703624117294, 23.48270179215985110, 11.16877607737301048 ) ) ;
#22035 = ORIENTED_EDGE ( 'NONE', *, *, #24365, .F. ) ;
#22036 = CARTESIAN_POINT ( 'NONE',  ( -3.999999999999997335, 27.45624999877096784, 11.30940107675849404 ) ) ;
#22037 = CARTESIAN_POINT ( 'NONE',  ( 3.999999999999996447, -27.92500000000000071, 8.999999999999992895 ) ) ;
#22039 = EDGE_LOOP ( 'NONE', ( #8545, #25147 ) ) ;
#22038 = CARTESIAN_POINT ( 'NONE',  ( -3.756430356250000546, 28.21562499938548996, 11.16877607737301048 ) ) ;
#22040 = CARTESIAN_POINT ( 'NONE',  ( -3.756430356249997438, 27.31562499938548427, 11.16877607737301048 ) ) ;
#22041 = CARTESIAN_POINT ( 'NONE',  ( -5.577813053751546416E-15, -25.73124999877096997, 12.99999999999999289 ) ) ;
#22042 = CARTESIAN_POINT ( 'NONE',  ( 3.834746474454188013E-15, 26.40624999877096357, 4.999999999999992006 ) ) ;
#22043 = ORIENTED_EDGE ( 'NONE', *, *, #20508, .T. ) ;
#22044 = ORIENTED_EDGE ( 'NONE', *, *, #23989, .F. ) ;
#22045 = LINE ( 'NONE', #21803, #6371 ) ;
#22046 = CARTESIAN_POINT ( 'NONE',  ( -2.003086131649545506E-15, 27.27812499938548640, 13.33755215474602984 ) ) ;
#22047 = DIRECTION ( 'NONE',  ( 0.2486898871648653975, 0.9685831611286285225, 0.000000000000000000 ) ) ;
#22048 = CARTESIAN_POINT ( 'NONE',  ( -3.756430356249996994, -8.999999999999992895, 3.965624999385481519 ) ) ;
#22049 = AXIS2_PLACEMENT_3D ( 'NONE', #11905, #19873, #7468 ) ;
#22050 = EDGE_CURVE ( 'NONE', #7760, #22793, #24739, .T. ) ;
#22051 = CARTESIAN_POINT ( 'NONE',  ( -3.999999999999997335, 27.45624999877096784, 11.30940107675849404 ) ) ;
#22052 = FILL_AREA_STYLE_COLOUR ( '', #12265 ) ;
#22053 = FACE_OUTER_BOUND ( 'NONE', #19978, .T. ) ;
#22054 = CARTESIAN_POINT ( 'NONE',  ( 6.938893903907228378E-15, 31.50000000000000000, 2.999999999999992450 ) ) ;
#22055 = CARTESIAN_POINT ( 'NONE',  ( 21.21320343559646915, 21.21320343559638744, 12.99999999999999289 ) ) ;
#22056 = AXIS2_PLACEMENT_3D ( 'NONE', #17161, #25262, #17414 ) ;
#22057 = CARTESIAN_POINT ( 'NONE',  ( 2.000000000000000888, 25.37500000000000000, 12.46410161513774817 ) ) ;
#22058 = CARTESIAN_POINT ( 'NONE',  ( -3.999999999999982681, -11.30940107675850292, 2.006249998770965437 ) ) ;
#22059 = CARTESIAN_POINT ( 'NONE',  ( 17.51415108564528467, 23.17100533513759331, 8.999999999999992895 ) ) ;
#22060 = ORIENTED_EDGE ( 'NONE', *, *, #13506, .T. ) ;
#22061 = CARTESIAN_POINT ( 'NONE',  ( 1.999999999999998224, -27.10000000000000142, 12.46410161513774639 ) ) ;
#22062 = CARTESIAN_POINT ( 'NONE',  ( 2.444316569969958497, 29.90105888194226580, 5.822820249163556561 ) ) ;
#22063 = CARTESIAN_POINT ( 'NONE',  ( 2.672651547586948120E-15, 29.64062499938548356, 13.33755215474602984 ) ) ;
#22064 = CARTESIAN_POINT ( 'NONE',  ( -3.999999999999949818, -6.690598923241462437, 2.437499999999999112 ) ) ;
#22065 = CARTESIAN_POINT ( 'NONE',  ( -1.071796769724485232, 26.03259618943233988, 4.999999999999992006 ) ) ;
#22066 = DIRECTION ( 'NONE',  ( -0.000000000000000000, -0.000000000000000000, -1.000000000000000000 ) ) ;
#22067 = VERTEX_POINT ( 'NONE', #10473 ) ;
#22068 = FACE_OUTER_BOUND ( 'NONE', #23494, .T. ) ;
#22069 = CARTESIAN_POINT ( 'NONE',  ( 2.000000000000000888, 26.21874999877096712, 12.46410161513774817 ) ) ;
#22070 = CYLINDRICAL_SURFACE ( 'NONE', #6263, 31.10000000000000142 ) ;
#22072 = VERTEX_POINT ( 'NONE', #18981 ) ;
#22071 = PLANE ( 'NONE',  #9160 ) ;
#22073 = AXIS2_PLACEMENT_3D ( 'NONE', #20105, #4535, #14099 ) ;
#22074 = EDGE_LOOP ( 'NONE', ( #10950, #15242, #16043, #10256 ) ) ;
#22075 = ORIENTED_EDGE ( 'NONE', *, *, #15359, .T. ) ;
#22076 = AXIS2_PLACEMENT_3D ( 'NONE', #3989, #9997, #17991 ) ;
#22077 = EDGE_LOOP ( 'NONE', ( #16791, #3779, #5933, #22311, #19498, #8255, #17019, #18898, #4723, #16865, #6782, #21862, #12696, #4934, #19768, #166, #7325, #23811, #1241, #3941, #8526, #9442, #12428, #2846 ) ) ;
#22078 = DIRECTION ( 'NONE',  ( 0.9921147013144794302, 0.1253332335642911299, 0.000000000000000000 ) ) ;
#22079 = CARTESIAN_POINT ( 'NONE',  ( -1.878215178124998275, 26.30312499938548854, 5.746835883940462963 ) ) ;
#22080 = CIRCLE ( 'NONE', #10792, 31.10000000000000142 ) ;
#22081 = MANIFOLD_SOLID_BREP ( 'Boss-Extrude2', #14639 ) ;
#22082 = CARTESIAN_POINT ( 'NONE',  ( -1.999999999999995781, 26.44374999877096855, 5.535898384862237620 ) ) ;
#22083 = CARTESIAN_POINT ( 'NONE',  ( -1.878215178124996498, 27.09062499938548996, 5.746835883940462963 ) ) ;
#22084 = DIRECTION ( 'NONE',  ( 0.9822872507286911636, 0.1873813145857119722, 0.000000000000000000 ) ) ;
#22085 = CARTESIAN_POINT ( 'NONE',  ( 4.000000000000003553, -8.999999999999992895, 3.543749998770967302 ) ) ;
#22086 = CARTESIAN_POINT ( 'NONE',  ( 3.735045420075836212E-15, 26.15312499938548285, 4.662447845253954171 ) ) ;
#22087 = ADVANCED_FACE ( 'NONE', ( #24868, #22900 ), #24596, .T. ) ;
#22088 = FACE_OUTER_BOUND ( 'NONE', #23915, .T. ) ;
#22089 = CARTESIAN_POINT ( 'NONE',  ( 0.7500000000000000000, 0.000000000000000000, 17.69999999999999929 ) ) ;
#22090 = CARTESIAN_POINT ( 'NONE',  ( -1.878215178124995832, 26.64062499938548711, 5.746835883940462963 ) ) ;
#22091 = LINE ( 'NONE', #14396, #3368 ) ;
#22092 = CARTESIAN_POINT ( 'NONE',  ( 30.85476721088025442, -3.897863563849982782, 1.000000000000000000 ) ) ;
#22093 = CARTESIAN_POINT ( 'NONE',  ( 0.000000000000000000, 0.000000000000000000, -6.500000000000000000 ) ) ;
#22094 = EDGE_CURVE ( 'NONE', #2636, #21178, #21304, .T. ) ;
#22095 = CARTESIAN_POINT ( 'NONE',  ( -2.000000000000003997, -28.16874999877096997, 5.535898384862238508 ) ) ;
#22096 = CARTESIAN_POINT ( 'NONE',  ( -3.756430356249996994, 29.07812499938548356, 8.999999999999992895 ) ) ;
#22097 = LINE ( 'NONE', #8246, #24139 ) ;
#22099 = CARTESIAN_POINT ( 'NONE',  ( -3.999999999999996447, -8.999999999999992895, 1.574999999999999956 ) ) ;
#22098 = CIRCLE ( 'NONE', #12479, 0.5000000000000002220 ) ;
#22100 = DIRECTION ( 'NONE',  ( 0.000000000000000000, 0.000000000000000000, -1.000000000000000000 ) ) ;
#22101 = ORIENTED_EDGE ( 'NONE', *, *, #9732, .F. ) ;
#22102 = EDGE_CURVE ( 'NONE', #19667, #10774, #6949, .T. ) ;
#22103 = CARTESIAN_POINT ( 'NONE',  ( 23.61528431363239022, 18.30288955771356640, 8.999999999999992895 ) ) ;
#22105 = VERTEX_POINT ( 'NONE', #18711 ) ;
#22104 = CARTESIAN_POINT ( 'NONE',  ( -1.499999999999998224, -7.499999999999992006, 0.000000000000000000 ) ) ;
#22106 = ORIENTED_EDGE ( 'NONE', *, *, #2035, .F. ) ;
#22107 = VECTOR ( 'NONE', #2681, 1000.000000000000000 ) ;
#22108 = VERTEX_POINT ( 'NONE', #803 ) ;
#22109 = ORIENTED_EDGE ( 'NONE', *, *, #5161, .T. ) ;
#22110 = ORIENTED_EDGE ( 'NONE', *, *, #23797, .T. ) ;
#22111 = CARTESIAN_POINT ( 'NONE',  ( 21.26623644418545211, 18.43780931943919299, 12.46410161513774817 ) ) ;
#22112 = CIRCLE ( 'NONE', #7093, 0.5000000000000006661 ) ;
#22113 = AXIS2_PLACEMENT_3D ( 'NONE', #12820, #3142, #17139 ) ;
#22114 = ORIENTED_EDGE ( 'NONE', *, *, #25110, .F. ) ;
#22115 = CARTESIAN_POINT ( 'NONE',  ( -1.999999999999998224, 29.35000000000000142, 12.46410161513774639 ) ) ;
#22116 = CARTESIAN_POINT ( 'NONE',  ( -1.878215178124995832, 25.40312499938548640, 5.746835883940462963 ) ) ;
#22117 = AXIS2_PLACEMENT_3D ( 'NONE', #5981, #17630, #21933 ) ;
#22118 = AXIS2_PLACEMENT_3D ( 'NONE', #2660, #20424, #18493 ) ;
#22119 =( REPRESENTATION_RELATIONSHIP ('NONE','NONE', #25031, #1120 ) REPRESENTATION_RELATIONSHIP_WITH_TRANSFORMATION ( #16002 )SHAPE_REPRESENTATION_RELATIONSHIP( ) );
#22120 = CARTESIAN_POINT ( 'NONE',  ( 3.756430356250002323, -11.16877607737301226, 3.815624999385482052 ) ) ;
#22121 = CARTESIAN_POINT ( 'NONE',  ( -27.92360179968386547, -13.69242354489123770, 1.000000000000000000 ) ) ;
#22122 = CARTESIAN_POINT ( 'NONE',  ( 19.68856820379214057, 17.03237082583270023, 12.25316411605952283 ) ) ;
#22123 =( BOUNDED_CURVE ( )  B_SPLINE_CURVE ( 2, ( #6526, #15028, #6916, #8624, #6653 ),
 .UNSPECIFIED., .F., .F. ) 
 B_SPLINE_CURVE_WITH_KNOTS ( ( 3, 2, 3 ),
 ( 0.000000000000000000, 0.01666666666666666644, 0.02500000000000000486 ),
 .UNSPECIFIED. ) 
 CURVE ( )  GEOMETRIC_REPRESENTATION_ITEM ( )  RATIONAL_B_SPLINE_CURVE ( ( 1.000000000000000000, 0.8660254037844387076, 1.000000000000000000, 0.9330127018922192983, 0.9330127018922194093 ) ) 
 REPRESENTATION_ITEM ( '' )  );
#22124 = DIRECTION ( 'NONE',  ( -0.000000000000000000, -1.000000000000000000, -0.000000000000000000 ) ) ;
#22125 =( LENGTH_UNIT ( ) NAMED_UNIT ( * ) SI_UNIT ( .MILLI., .METRE. ) );
#22126 = AXIS2_PLACEMENT_3D ( 'NONE', #10711, #4326, #24197 ) ;
#22127 = CARTESIAN_POINT ( 'NONE',  ( -1.878215178124995832, -5.746835883940462963, 0.7406249993854828739 ) ) ;
#22128 = CARTESIAN_POINT ( 'NONE',  ( 3.752267015613588906E-15, 27.81250000000000000, 4.381197846482986158 ) ) ;
#22129 = CARTESIAN_POINT ( 'NONE',  ( 3.735045420075836212E-15, 28.40312499938548640, 4.662447845253954171 ) ) ;
#22130 =( BOUNDED_CURVE ( )  B_SPLINE_CURVE ( 2, ( #1979, #11291, #4058, #25411, #5900, #7499, #13886, #3943, #9945 ),
 .UNSPECIFIED., .F., .F. ) 
 B_SPLINE_CURVE_WITH_KNOTS ( ( 3, 2, 2, 2, 3 ),
 ( 0.6750000000000000444, 0.6833333333333333481, 0.6999999999999999556, 0.7166666666666666741, 0.7249999999999999778 ),
 .UNSPECIFIED. ) 
 CURVE ( )  GEOMETRIC_REPRESENTATION_ITEM ( )  RATIONAL_B_SPLINE_CURVE ( ( 0.9330127018922194093, 0.9330127018922198534, 1.000000000000000000, 0.8660254037844387076, 1.000000000000000000, 0.8660254037844387076, 1.000000000000000000, 0.9330127018922194093, 0.9330127018922194093 ) ) 
 REPRESENTATION_ITEM ( '' )  );
#22131 = MECHANICAL_DESIGN_GEOMETRIC_PRESENTATION_REPRESENTATION (  '', ( #20016 ), #24630 ) ;
#22132 = DIRECTION ( 'NONE',  ( 1.000000000000000000, 0.000000000000000000, 0.000000000000000000 ) ) ;
#22133 = CARTESIAN_POINT ( 'NONE',  ( 16.75401129586974491, 19.58243842061586548, 12.46410161513774639 ) ) ;
#22134 = DIRECTION ( 'NONE',  ( 0.000000000000000000, 0.000000000000000000, 1.000000000000000000 ) ) ;
#22135 = EDGE_LOOP ( 'NONE', ( #6298, #8315, #16503, #2310 ) ) ;
#22136 = ADVANCED_FACE ( 'NONE', ( #8781 ), #20604, .T. ) ;
#22137 = ORIENTED_EDGE ( 'NONE', *, *, #17800, .T. ) ;
#22138 = CARTESIAN_POINT ( 'NONE',  ( 3.756430356250002323, 25.66562499938548925, 11.16877607737301226 ) ) ;
#22140 = EDGE_CURVE ( 'NONE', #21434, #10206, #3570, .T. ) ;
#22139 = VECTOR ( 'NONE', #20872, 1000.000000000000000 ) ;
#22141 = ORIENTED_EDGE ( 'NONE', *, *, #12112, .F. ) ;
#22142 = FACE_OUTER_BOUND ( 'NONE', #7712, .T. ) ;
#22143 = CARTESIAN_POINT ( 'NONE',  ( -1.878215178124998497, 26.00312499938548783, 12.25316411605951927 ) ) ;
#22144 = CARTESIAN_POINT ( 'NONE',  ( 15.60496277644160124, 21.26181702593391876, 8.999999999999992895 ) ) ;
#22145 = ORIENTED_EDGE ( 'NONE', *, *, #2909, .T. ) ;
#22146 = ADVANCED_FACE ( 'NONE', ( #3236 ), #3120, .T. ) ;
#22147 = CYLINDRICAL_SURFACE ( 'NONE', #2738, 0.5000000000000000000 ) ;
#22148 = AXIS2_PLACEMENT_3D ( 'NONE', #21761, #23850, #25559 ) ;
#22149 = VERTEX_POINT ( 'NONE', #9126 ) ;
#22150 = CARTESIAN_POINT ( 'NONE',  ( -0.4995657836784084815, 38.49999999999999289, 14.97916666666665897 ) ) ;
#22151 = CARTESIAN_POINT ( 'NONE',  ( 2.672651547586948120E-15, 27.72812499938548569, 13.33755215474602984 ) ) ;
#22152 = DIRECTION ( 'NONE',  ( 0.000000000000000000, 0.000000000000000000, 1.000000000000000000 ) ) ;
#22153 = AXIS2_PLACEMENT_3D ( 'NONE', #8508, #16489, #10311 ) ;
#22154 = VECTOR ( 'NONE', #5825, 1000.000000000000000 ) ;
#22155 = EDGE_CURVE ( 'NONE', #3259, #12818, #19189, .T. ) ;
#22156 = FACE_OUTER_BOUND ( 'NONE', #20174, .T. ) ;
#22157 = DIRECTION ( 'NONE',  ( -0.000000000000000000, -0.000000000000000000, 1.000000000000000000 ) ) ;
#22158 = CARTESIAN_POINT ( 'NONE',  ( -3.999999999999999556, 28.41250000000000142, 11.30940107675849404 ) ) ;
#22159 = CIRCLE ( 'NONE', #23823, 6.000000000000000000 ) ;
#22160 = DIRECTION ( 'NONE',  ( 0.000000000000000000, 0.000000000000000000, -1.000000000000000000 ) ) ;
#22161 = CARTESIAN_POINT ( 'NONE',  ( -1.859271017917182139E-15, -28.88124999877096499, 12.99999999999999289 ) ) ;
#22162 = AXIS2_PLACEMENT_3D ( 'NONE', #7929, #13685, #21658 ) ;
#22163 = EDGE_CURVE ( 'NONE', #11427, #13061, #10421, .T. ) ;
#22164 = CARTESIAN_POINT ( 'NONE',  ( -30.45149776762720961, 6.317933499823766397, -6.500000000000000000 ) ) ;
#22165 = PRODUCT_DEFINITION_SHAPE ( 'NONE', 'NONE',  #10273 ) ;
#22166 = CARTESIAN_POINT ( 'NONE',  ( 19.60447174239884305, 22.26066912035814127, 12.25316411605951927 ) ) ;
#22167 = DIRECTION ( 'NONE',  ( 1.000000000000000000, 0.000000000000000000, 0.000000000000000000 ) ) ;
#22168 = CIRCLE ( 'NONE', #15925, 0.5000000000000001110 ) ;
#22170 = EDGE_CURVE ( 'NONE', #18613, #22942, #8934, .T. ) ;
#22169 = CARTESIAN_POINT ( 'NONE',  ( -3.756430356250003211, -25.62812499938548072, 6.831223922626973533 ) ) ;
#22171 = VECTOR ( 'NONE', #16994, 1000.000000000000000 ) ;
#22172 = CARTESIAN_POINT ( 'NONE',  ( 27.09999999999999787, -0.5999999999999998668, 19.59999999999999787 ) ) ;
#22173 = ORIENTED_EDGE ( 'NONE', *, *, #5089, .T. ) ;
#22174 = CARTESIAN_POINT ( 'NONE',  ( 4.000000000000003553, 27.23124999877096997, 6.690598923241489970 ) ) ;
#22175 = CARTESIAN_POINT ( 'NONE',  ( -3.752267015613588906E-15, -28.26250000000000284, 4.381197846482986158 ) ) ;
#22177 = ORIENTED_EDGE ( 'NONE', *, *, #24202, .F. ) ;
#22176 = CARTESIAN_POINT ( 'NONE',  ( 3.756430356250004987, 27.95312499938548711, 8.999999999999992895 ) ) ;
#22178 = VECTOR ( 'NONE', #13023, 1000.000000000000000 ) ;
#22179 = CARTESIAN_POINT ( 'NONE',  ( -1.878215178124995832, 29.00312499938548427, 5.746835883940462963 ) ) ;
#22180 = AXIS2_PLACEMENT_3D ( 'NONE', #9396, #11598, #17378 ) ;
#22181 = FACE_OUTER_BOUND ( 'NONE', #24405, .T. ) ;
#22182 = DIRECTION ( 'NONE',  ( -0.000000000000000000, -0.000000000000000000, -1.000000000000000000 ) ) ;
#22183 = ORIENTED_EDGE ( 'NONE', *, *, #22021, .F. ) ;
#22184 = EDGE_LOOP ( 'NONE', ( #6038, #1019, #7620, #12450 ) ) ;
#22185 = CARTESIAN_POINT ( 'NONE',  ( 3.756430356249996994, -25.92812499938548498, 8.999999999999992895 ) ) ;
#22186 = CARTESIAN_POINT ( 'NONE',  ( 8.012344526598182026E-15, 28.85312499938549280, 4.662447845253954171 ) ) ;
#22187 = CARTESIAN_POINT ( 'NONE',  ( 22.05731215476884088, 16.40045790527639369, 8.999999999999992895 ) ) ;
#22188 = EDGE_CURVE ( 'NONE', #18705, #4416, #3754, .T. ) ;
#22189 = AXIS2_PLACEMENT_3D ( 'NONE', #10362, #6462, #8431 ) ;
#22190 = CARTESIAN_POINT ( 'NONE',  ( 1.878215178125000939, -12.25316411605952283, 3.665624999385483473 ) ) ;
#22191 = CIRCLE ( 'NONE', #12161, 0.4999999999999997224 ) ;
#22192 = AXIS2_PLACEMENT_3D ( 'NONE', #8082, #10158, #17883 ) ;
#22193 = DIRECTION ( 'NONE',  ( 0.000000000000000000, -0.000000000000000000, 1.000000000000000000 ) ) ;
#22194 = CARTESIAN_POINT ( 'NONE',  ( 4.000000000000003553, -8.999999999999992895, 2.249999999999998668 ) ) ;
#22195 = VECTOR ( 'NONE', #6494, 1000.000000000000000 ) ;
#22196 = FACE_OUTER_BOUND ( 'NONE', #12561, .T. ) ;
#22197 = CARTESIAN_POINT ( 'NONE',  ( 18.68840298406382416, 17.17265345621170169, 12.99999999999999467 ) ) ;
#22198 = CARTESIAN_POINT ( 'NONE',  ( -1.071796769724485676, 26.61115380933863861, 12.99999999999999467 ) ) ;
#22199 = CARTESIAN_POINT ( 'NONE',  ( 21.70609600442870857, 16.39370124850988830, 8.999999999999992895 ) ) ;
#22200 = CARTESIAN_POINT ( 'NONE',  ( 17.54066758993977970, 23.19752183943208479, 11.30940107675849404 ) ) ;
#22201 = VERTEX_POINT ( 'NONE', #21671 ) ;
#22202 = CARTESIAN_POINT ( 'NONE',  ( 1.500000000000001776, -7.499999999999993783, 30.00000000000000355 ) ) ;
#22203 = CARTESIAN_POINT ( 'NONE',  ( -28.14012133169306296, 13.24173596767408867, -6.500000000000000000 ) ) ;
#22204 = CARTESIAN_POINT ( 'NONE',  ( 2.672651547586948120E-15, 25.92812499938548498, 13.33755215474602984 ) ) ;
#22206 = ORIENTED_EDGE ( 'NONE', *, *, #24626, .T. ) ;
#22205 = CARTESIAN_POINT ( 'NONE',  ( -3.180741987853693331, 29.83126030492351788, 11.43940974718624837 ) ) ;
#22207 = CIRCLE ( 'NONE', #13865, 31.10000000000000142 ) ;
#22208 = DIRECTION ( 'NONE',  ( 0.000000000000000000, 0.000000000000000000, 1.000000000000000000 ) ) ;
#22209 = CARTESIAN_POINT ( 'NONE',  ( -3.834746474454188013E-15, -27.81249999999999645, 4.999999999999992006 ) ) ;
#22210 = ORIENTED_EDGE ( 'NONE', *, *, #12498, .F. ) ;
#22211 = DIRECTION ( 'NONE',  ( 0.000000000000000000, -1.000000000000000000, 0.000000000000000000 ) ) ;
#22212 = CARTESIAN_POINT ( 'NONE',  ( 2.000000000000003997, 25.46874999877096712, 5.535898384862238508 ) ) ;
#22213 = CARTESIAN_POINT ( 'NONE',  ( -3.756430356250002323, -26.00312499938548427, 11.16877607737301226 ) ) ;
#22215 = ORIENTED_EDGE ( 'NONE', *, *, #24972, .F. ) ;
#22214 = CARTESIAN_POINT ( 'NONE',  ( 27.09999999999999787, -0.5999999999999998668, 19.59999999999999787 ) ) ;
#22216 = EDGE_CURVE ( 'NONE', #16526, #15841, #2574, .T. ) ;
#22217 = ORIENTED_EDGE ( 'NONE', *, *, #4434, .F. ) ;
#22218 = EDGE_LOOP ( 'NONE', ( #11655, #16591, #4302, #12705 ) ) ;
#22219 = VERTEX_POINT ( 'NONE', #13963 ) ;
#22220 = CARTESIAN_POINT ( 'NONE',  ( 12.78762572734057024, 28.34936733434201273, -6.500000000000000000 ) ) ;
#22222 = CARTESIAN_POINT ( 'NONE',  ( 3.756430356250004543, 25.74062499938548498, 6.831223922626973533 ) ) ;
#22221 = CIRCLE ( 'NONE', #7176, 31.10000000000000142 ) ;
#22223 = FILL_AREA_STYLE ('',( #12006 ) ) ;
#22224 = AXIS2_PLACEMENT_3D ( 'NONE', #14413, #24588, #2497 ) ;
#22225 = CARTESIAN_POINT ( 'NONE',  ( -3.999999999999996447, 28.86250000000000071, 11.30940107675849404 ) ) ;
#22226 = CARTESIAN_POINT ( 'NONE',  ( 2.000000000000000888, -12.46410161513774817, 4.818749998770965881 ) ) ;
#22227 = VECTOR ( 'NONE', #23900, 1000.000000000000000 ) ;
#22228 = CARTESIAN_POINT ( 'NONE',  ( 3.756430356250002323, 26.90312499938548640, 11.16877607737301226 ) ) ;
#22229 = AXIS2_PLACEMENT_3D ( 'NONE', #22629, #20135, #14128 ) ;
#22230 = DIRECTION ( 'NONE',  ( 0.000000000000000000, 0.000000000000000000, 1.000000000000000000 ) ) ;
#22231 = CYLINDRICAL_SURFACE ( 'NONE', #23063, 31.10000000000000142 ) ;
#22232 = CARTESIAN_POINT ( 'NONE',  ( 2.672651547586948120E-15, 25.47812499938548569, 13.33755215474603162 ) ) ;
#22233 = DIRECTION ( 'NONE',  ( 1.000000000000000000, 0.000000000000000000, 0.000000000000000000 ) ) ;
#22234 = CARTESIAN_POINT ( 'NONE',  ( 0.000000000000000000, -31.10000000000000142, -6.500000000000000000 ) ) ;
#22235 = DIRECTION ( 'NONE',  ( 0.000000000000000000, 0.000000000000000000, 1.000000000000000000 ) ) ;
#22236 = CARTESIAN_POINT ( 'NONE',  ( -3.752267015613588906E-15, -29.10624999877096997, 4.381197846482986158 ) ) ;
#22237 = CARTESIAN_POINT ( 'NONE',  ( 10.08469938919477649, -29.41953157733097868, -6.500000000000000000 ) ) ;
#22238 = CARTESIAN_POINT ( 'NONE',  ( -0.7500000000000000000, -1.299038105676658450, 18.19999999999999929 ) ) ;
#22239 = CARTESIAN_POINT ( 'NONE',  ( -3.999999999999996447, 29.66874999877096997, 8.999999999999992895 ) ) ;
#22240 = LINE ( 'NONE', #10319, #18914 ) ;
#22241 = VERTEX_POINT ( 'NONE', #21809 ) ;
#22242 = DIRECTION ( 'NONE',  ( 0.000000000000000000, 0.000000000000000000, 1.000000000000000000 ) ) ;
#22244 = ORIENTED_EDGE ( 'NONE', *, *, #6913, .F. ) ;
#22243 = CYLINDRICAL_SURFACE ( 'NONE', #25868, 0.5000000000000004441 ) ;
#22245 = AXIS2_PLACEMENT_3D ( 'NONE', #13719, #24172, #7969 ) ;
#22247 = ORIENTED_EDGE ( 'NONE', *, *, #24156, .F. ) ;
#22246 = EDGE_CURVE ( 'NONE', #18764, #6939, #11978, .T. ) ;
#22248 = ORIENTED_EDGE ( 'NONE', *, *, #20430, .T. ) ;
#22249 = VERTEX_POINT ( 'NONE', #13694 ) ;
#22250 = EDGE_LOOP ( 'NONE', ( #10912, #6570, #6112, #21603, #21915 ) ) ;
#22251 = EDGE_LOOP ( 'NONE', ( #25040, #17975, #19089, #8339 ) ) ;
#22252 = AXIS2_PLACEMENT_3D ( 'NONE', #14820, #22792, #21475 ) ;
#22253 = ADVANCED_FACE ( 'NONE', ( #108 ), #1931, .T. ) ;
#22254 = ORIENTED_EDGE ( 'NONE', *, *, #24592, .T. ) ;
#22255 = EDGE_CURVE ( 'NONE', #25532, #9390, #12526, .T. ) ;
#22256 = DIRECTION ( 'NONE',  ( 1.000000000000000000, 0.000000000000000000, 0.000000000000000000 ) ) ;
#22257 = CARTESIAN_POINT ( 'NONE',  ( -1.878215178124998497, 26.90312499938548285, 12.25316411605951927 ) ) ;
#22258 = VECTOR ( 'NONE', #10754, 1000.000000000000000 ) ;
#22259 = CARTESIAN_POINT ( 'NONE',  ( 2.672651547586948120E-15, -13.33755215474602984, 3.290624999385483918 ) ) ;
#22260 = CARTESIAN_POINT ( 'NONE',  ( 4.000000000000007105, 25.93750000000000711, 6.690598923241489970 ) ) ;
#22261 = CARTESIAN_POINT ( 'NONE',  ( 21.04318339706631846, 15.73078864114750530, 11.16877607737301226 ) ) ;
#22262 = EDGE_CURVE ( 'NONE', #22434, #15016, #4592, .T. ) ;
#22263 = DIRECTION ( 'NONE',  ( 0.000000000000000000, 0.000000000000000000, -1.000000000000000000 ) ) ;
#22264 = AXIS2_PLACEMENT_3D ( 'NONE', #16800, #2923, #1706 ) ;
#22265 = CARTESIAN_POINT ( 'NONE',  ( -20.20656826142249685, 23.64116323484259752, -6.500000000000000000 ) ) ;
#22266 = CARTESIAN_POINT ( 'NONE',  ( 2.672651547586948120E-15, -13.33755215474602984, 2.278124999385481519 ) ) ;
#22267 = CARTESIAN_POINT ( 'NONE',  ( -28.91604871112473418, -11.44867358849319849, -6.500000000000000000 ) ) ;
#22268 = CARTESIAN_POINT ( 'NONE',  ( -3.756430356249996105, 28.47812499938548569, 6.831223922626973533 ) ) ;
#22269 = CARTESIAN_POINT ( 'NONE',  ( -3.756430356249996105, -6.831223922626973533, 1.790624999385485028 ) ) ;
#22270 = DIRECTION ( 'NONE',  ( 0.000000000000000000, -1.000000000000000000, 0.000000000000000000 ) ) ;
#22271 = FACE_OUTER_BOUND ( 'NONE', #2107, .T. ) ;
#22272 = VERTEX_POINT ( 'NONE', #9893 ) ;
#22273 = VERTEX_POINT ( 'NONE', #19710 ) ;
#22274 = CARTESIAN_POINT ( 'NONE',  ( -1.878215178124999829, 27.80312499938548854, 12.25316411605951927 ) ) ;
#22275 = ORIENTED_EDGE ( 'NONE', *, *, #13998, .T. ) ;
#22276 = FACE_OUTER_BOUND ( 'NONE', #6874, .T. ) ;
#22277 = COLOUR_RGB ( '',0.8941176470588234615, 0.8941176470588234615, 0.8941176470588234615 ) ;
#22278 = VERTEX_POINT ( 'NONE', #17880 ) ;
#22279 = DIRECTION ( 'NONE',  ( 1.000000000000000000, 0.000000000000000000, 0.000000000000000000 ) ) ;
#22280 = ORIENTED_EDGE ( 'NONE', *, *, #16411, .T. ) ;
#22281 = ADVANCED_FACE ( 'NONE', ( #14084 ), #23899, .F. ) ;
#22282 = DIRECTION ( 'NONE',  ( 0.000000000000000000, 0.000000000000000000, 1.000000000000000000 ) ) ;
#22283 = ORIENTED_EDGE ( 'NONE', *, *, #12825, .T. ) ;
#22284 = PRODUCT_DEFINITION ( 'UNKNOWN', '', #8973, #16995 ) ;
#22285 = CARTESIAN_POINT ( 'NONE',  ( 0.000000000000000000, 0.000000000000000000, -6.500000000000000000 ) ) ;
#22286 =( BOUNDED_CURVE ( )  B_SPLINE_CURVE ( 2, ( #2071, #15942, #23913, #5996, #9665, #17648, #25619, #13978, #21947 ),
 .UNSPECIFIED., .F., .F. ) 
 B_SPLINE_CURVE_WITH_KNOTS ( ( 3, 2, 2, 2, 3 ),
 ( 0.2250000000000000056, 0.2333333333333333370, 0.2500000000000000000, 0.2666666666666666630, 0.2750000000000000222 ),
 .UNSPECIFIED. ) 
 CURVE ( )  GEOMETRIC_REPRESENTATION_ITEM ( )  RATIONAL_B_SPLINE_CURVE ( ( 0.9330127018922194093, 0.9330127018922194093, 1.000000000000000000, 0.8660254037844387076, 1.000000000000000000, 0.8660254037844387076, 1.000000000000000000, 0.9330127018922191873, 0.9330127018922194093 ) ) 
 REPRESENTATION_ITEM ( '' )  );
#22287 = CARTESIAN_POINT ( 'NONE',  ( 3.756430356250003655, 28.29062499938548569, 8.999999999999992895 ) ) ;
#22288 = DIRECTION ( 'NONE',  ( 0.000000000000000000, 0.000000000000000000, 1.000000000000000000 ) ) ;
#22289 = CARTESIAN_POINT ( 'NONE',  ( 2.000000000000003997, 26.87500000000000355, 5.535898384862238508 ) ) ;
#22290 = CARTESIAN_POINT ( 'NONE',  ( 1.500000000000001776, -10.49999999999999289, 30.00000000000000355 ) ) ;
#22291 = CARTESIAN_POINT ( 'NONE',  ( 4.000000000000000888, 28.63750000000000639, 6.690598923241489970 ) ) ;
#22292 = ADVANCED_FACE ( 'NONE', ( #9647 ), #7939, .F. ) ;
#22293 =( BOUNDED_CURVE ( )  B_SPLINE_CURVE ( 2, ( #1589, #19241, #15207, #20962, #21087, #17169, #13236 ),
 .UNSPECIFIED., .F., .F. ) 
 B_SPLINE_CURVE_WITH_KNOTS ( ( 3, 2, 2, 3 ),
 ( 0.7999999999999999334, 0.8166666666666665408, 0.8333333333333332593, 0.8499999999999998668 ),
 .UNSPECIFIED. ) 
 CURVE ( )  GEOMETRIC_REPRESENTATION_ITEM ( )  RATIONAL_B_SPLINE_CURVE ( ( 1.000000000000000888, 0.8660254037844378194, 1.000000000000000000, 0.8660254037844387076, 1.000000000000000000, 0.8660254037844395958, 0.9999999999999991118 ) ) 
 REPRESENTATION_ITEM ( '' )  );
#22294 = EDGE_CURVE ( 'NONE', #15214, #10411, #15872, .T. ) ;
#22295 = STYLED_ITEM ( 'NONE', ( #12252 ), #21253 ) ;
#22296 = CARTESIAN_POINT ( 'NONE',  ( 3.756430356250002323, 27.35312499938547859, 11.16877607737301226 ) ) ;
#22297 = CARTESIAN_POINT ( 'NONE',  ( -5.335677986745010593, -30.63887302793242284, -2.750000000000000000 ) ) ;
#22298 = VECTOR ( 'NONE', #5184, 1000.000000000000000 ) ;
#22299 = CARTESIAN_POINT ( 'NONE',  ( -0.2827178117968723869, 38.91165577845126222, 3.418461308658551356 ) ) ;
#22300 = DIRECTION ( 'NONE',  ( 0.000000000000000000, 0.000000000000000000, 1.000000000000000000 ) ) ;
#22301 = CARTESIAN_POINT ( 'NONE',  ( 3.469446951953614189E-15, 30.00000000000000355, 8.999999999999992895 ) ) ;
#22302 = ORIENTED_EDGE ( 'NONE', *, *, #22262, .F. ) ;
#22303 = CARTESIAN_POINT ( 'NONE',  ( -1.999999999999998224, 27.94374999877096855, 12.46410161513774639 ) ) ;
#22304 = CARTESIAN_POINT ( 'NONE',  ( -3.752267015613588906E-15, -28.71250000000000568, 4.381197846482986158 ) ) ;
#22306 = ORIENTED_EDGE ( 'NONE', *, *, #16401, .T. ) ;
#22305 = CARTESIAN_POINT ( 'NONE',  ( -3.756430356249994329, 26.86562499938548498, 11.16877607737301048 ) ) ;
#22307 = ORIENTED_EDGE ( 'NONE', *, *, #22411, .T. ) ;
#22308 = CARTESIAN_POINT ( 'NONE',  ( -3.999999999999997335, 28.80624999877096926, 11.30940107675849404 ) ) ;
#22309 = DIRECTION ( 'NONE',  ( -0.06279051952931542779, -0.9980267284282714479, 0.000000000000000000 ) ) ;
#22310 = CARTESIAN_POINT ( 'NONE',  ( -1.999999999999998224, 27.94374999877096855, 12.46410161513774639 ) ) ;
#22311 = ORIENTED_EDGE ( 'NONE', *, *, #20840, .F. ) ;
#22312 = VERTEX_POINT ( 'NONE', #4011 ) ;
#22313 = CARTESIAN_POINT ( 'NONE',  ( -1.878215178125000939, -27.42812499938548498, 12.25316411605952283 ) ) ;
#22314 = CARTESIAN_POINT ( 'NONE',  ( 3.756430356250006319, 26.97812499938548569, 6.831223922626973533 ) ) ;
#22315 = DIRECTION ( 'NONE',  ( 0.000000000000000000, -1.000000000000000000, 0.000000000000000000 ) ) ;
#22316 = EDGE_CURVE ( 'NONE', #7827, #19442, #10021, .T. ) ;
#22317 = CARTESIAN_POINT ( 'NONE',  ( 2.000000000000005329, 26.42500000000000426, 5.535898384862238508 ) ) ;
#22318 = EDGE_CURVE ( 'NONE', #14822, #23126, #25602, .T. ) ;
#22319 = DIRECTION ( 'NONE',  ( 0.000000000000000000, 0.000000000000000000, 1.000000000000000000 ) ) ;
#22320 = CARTESIAN_POINT ( 'NONE',  ( 1.071796769724488563, -28.46740381056766722, 12.99999999999999289 ) ) ;
#22321 = DIRECTION ( 'NONE',  ( 0.000000000000000000, -0.000000000000000000, -1.000000000000000000 ) ) ;
#22322 = CARTESIAN_POINT ( 'NONE',  ( 1.057460391440397258E-14, -29.55624999877096926, 4.999999999999992006 ) ) ;
#22323 = CARTESIAN_POINT ( 'NONE',  ( 4.000000000000003553, 25.48750000000000071, 6.690598923241489970 ) ) ;
#22324 = CARTESIAN_POINT ( 'NONE',  ( 17.19146985159974150, 19.84766722955904683, 5.746835883940462963 ) ) ;
#22325 = CARTESIAN_POINT ( 'NONE',  ( 22.98538980507618845, 17.32853555558373060, 11.30940107675849760 ) ) ;
#22326 = ORIENTED_EDGE ( 'NONE', *, *, #15640, .F. ) ;
#22327 = CYLINDRICAL_SURFACE ( 'NONE', #948, 6.000000000000000888 ) ;
#22328 = CARTESIAN_POINT ( 'NONE',  ( 1.775433037296146654, 29.94838521766437722, 5.406171146379000092 ) ) ;
#22329 = CARTESIAN_POINT ( 'NONE',  ( -3.756430356249995661, 25.77812499938548640, 6.831223922626973533 ) ) ;
#22331 = ORIENTED_EDGE ( 'NONE', *, *, #5915, .F. ) ;
#22330 = CARTESIAN_POINT ( 'NONE',  ( -2.644755406393140440, 29.88376691385261097, 5.987824696368042154 ) ) ;
#22332 = CARTESIAN_POINT ( 'NONE',  ( 18.17485398475098535, 18.17485398475091785, 4.662447845253954171 ) ) ;
#22333 = CARTESIAN_POINT ( 'NONE',  ( 2.620986760973688460E-15, -13.61880215351699874, 1.237499999999996270 ) ) ;
#22334 = ORIENTED_EDGE ( 'NONE', *, *, #3063, .T. ) ;
#22335 = CARTESIAN_POINT ( 'NONE',  ( 0.000000000000000000, 0.000000000000000000, 15.00000000000000178 ) ) ;
#22336 = CARTESIAN_POINT ( 'NONE',  ( -3.999999999999997335, 26.55624999877096926, 11.30940107675849404 ) ) ;
#22337 = CARTESIAN_POINT ( 'NONE',  ( -2.672651547586948120E-15, -25.92812499938548498, 13.33755215474602984 ) ) ;
#22339 = EDGE_LOOP ( 'NONE', ( #17450, #2659, #12987, #7227 ) ) ;
#22338 = CARTESIAN_POINT ( 'NONE',  ( -1.071796769724487230, 25.13259618943233420, 4.999999999999992006 ) ) ;
#22340 = VERTEX_POINT ( 'NONE', #1811 ) ;
#22341 = CARTESIAN_POINT ( 'NONE',  ( -2.672651547586948120E-15, -29.64062499938548356, 13.33755215474602984 ) ) ;
#22342 = ORIENTED_EDGE ( 'NONE', *, *, #18426, .F. ) ;
#22343 = ORIENTED_EDGE ( 'NONE', *, *, #7762, .F. ) ;
#22344 = CARTESIAN_POINT ( 'NONE',  ( 0.000000000000000000, 0.000000000000000000, 18.19999999999999929 ) ) ;
#22345 = CARTESIAN_POINT ( 'NONE',  ( 3.756430356250000546, 26.56562499938548783, 11.16877607737301226 ) ) ;
#22346 = ADVANCED_FACE ( 'NONE', ( #12643 ), #20475, .T. ) ;
#22347 = CARTESIAN_POINT ( 'NONE',  ( -3.756430356249997882, -11.16877607737301226, 1.415624999385483029 ) ) ;
#22348 = PRESENTATION_STYLE_ASSIGNMENT (( #15965 ) ) ;
#22349 = CARTESIAN_POINT ( 'NONE',  ( -3.756430356249997882, 27.20312499938548001, 11.16877607737301226 ) ) ;
#22350 = EDGE_CURVE ( 'NONE', #9107, #13049, #23133, .T. ) ;
#22351 = CARTESIAN_POINT ( 'NONE',  ( -20.92219106202066925, -23.01025686871623321, 1.000000000000000000 ) ) ;
#22352 = CARTESIAN_POINT ( 'NONE',  ( -3.999999999999996447, -8.999999999999992895, 3.824999999999998401 ) ) ;
#22353 = CARTESIAN_POINT ( 'NONE',  ( 3.756430356250003211, 26.07812499938548356, 6.831223922626973533 ) ) ;
#22354 = CARTESIAN_POINT ( 'NONE',  ( 16.66421332384664566, -26.25859848311276679, 1.000000000000000000 ) ) ;
#22355 = CARTESIAN_POINT ( 'NONE',  ( -3.526711513754876570, 31.50000000000000000, 4.145898033750337497 ) ) ;
#22356 = CARTESIAN_POINT ( 'NONE',  ( 1.859271017917182139E-15, 29.78124999877096712, 12.99999999999999289 ) ) ;
#22357 = CARTESIAN_POINT ( 'NONE',  ( 3.999999999999996003, -28.28124999877096712, 6.690598923241487306 ) ) ;
#22358 = CARTESIAN_POINT ( 'NONE',  ( 5.112995299272250684E-15, 27.36250000000000426, 4.999999999999992006 ) ) ;
#22360 = ADVANCED_FACE ( 'NONE', ( #8464 ), #24283, .F. ) ;
#22359 = LINE ( 'NONE', #4572, #1604 ) ;
#22361 = DIRECTION ( 'NONE',  ( 0.000000000000000000, 0.000000000000000000, 1.000000000000000000 ) ) ;
#22362 = FACE_OUTER_BOUND ( 'NONE', #24103, .T. ) ;
#22363 = EDGE_LOOP ( 'NONE', ( #9915, #13242, #9802 ) ) ;
#22364 = LINE ( 'NONE', #547, #10848 ) ;
#22366 = ORIENTED_EDGE ( 'NONE', *, *, #8966, .T. ) ;
#22365 = CARTESIAN_POINT ( 'NONE',  ( -5.335677986745010593, -30.63887302793242284, 1.000000000000000000 ) ) ;
#22367 = ORIENTED_EDGE ( 'NONE', *, *, #15274, .F. ) ;
#22368 = ORIENTED_EDGE ( 'NONE', *, *, #14009, .F. ) ;
#22369 = EDGE_LOOP ( 'NONE', ( #7062, #20506, #7064, #2878 ) ) ;
#22370 = VERTEX_POINT ( 'NONE', #24414 ) ;
#22371 = VERTEX_POINT ( 'NONE', #22441 ) ;
#22372 = DIRECTION ( 'NONE',  ( 1.000000000000000000, 0.000000000000000000, 0.000000000000000000 ) ) ;
#22373 = VERTEX_POINT ( 'NONE', #16312 ) ;
#22374 = CIRCLE ( 'NONE', #14452, 0.4999999999999998335 ) ;
#22375 = CARTESIAN_POINT ( 'NONE',  ( 2.000000000000003997, 28.67500000000000426, 5.535898384862238508 ) ) ;
#22376 = CARTESIAN_POINT ( 'NONE',  ( 3.735045420075836212E-15, 25.36562499938548854, 4.662447845253954171 ) ) ;
#22377 = CARTESIAN_POINT ( 'NONE',  ( 3.756430356250003655, -8.999999999999992895, 3.853124999385483473 ) ) ;
#22378 = CARTESIAN_POINT ( 'NONE',  ( 0.000000000000000000, 0.000000000000000000, 20.00000000000000000 ) ) ;
#22379 = PRODUCT ( 'dust cap', 'dust cap', '', ( #3337 ) ) ;
#22380 = CARTESIAN_POINT ( 'NONE',  ( 16.97933781724378122, 19.63553519520309010, 12.25316411605951927 ) ) ;
#22381 = CARTESIAN_POINT ( 'NONE',  ( -1.499999999999998224, -10.49999999999999289, 4.999999999999993783 ) ) ;
#22382 = EDGE_CURVE ( 'NONE', #10226, #13593, #20435, .T. ) ;
#22383 = DIRECTION ( 'NONE',  ( 0.000000000000000000, 1.000000000000000000, -0.000000000000000000 ) ) ;
#22384 = CARTESIAN_POINT ( 'NONE',  ( -3.756430356249996994, -8.999999999999992895, 1.265624999385484006 ) ) ;
#22385 = CARTESIAN_POINT ( 'NONE',  ( -1.999999999999998224, 27.94374999877096855, 12.46410161513774639 ) ) ;
#22386 = DIRECTION ( 'NONE',  ( -0.3681245526846659843, 0.9297764858882561212, 0.000000000000000000 ) ) ;
#22387 = CARTESIAN_POINT ( 'NONE',  ( 3.756430356250002323, 29.15312499938548640, 11.16877607737301403 ) ) ;
#22388 = CARTESIAN_POINT ( 'NONE',  ( 1.878215178125004048, -5.746835883940462963, 1.678124999385483651 ) ) ;
#22389 = ADVANCED_FACE ( 'NONE', ( #24664 ), #12501, .F. ) ;
#22390 = FACE_OUTER_BOUND ( 'NONE', #6474, .T. ) ;
#22391 = DIRECTION ( 'NONE',  ( 1.000000000000000000, 0.000000000000000000, 0.000000000000000000 ) ) ;
#22392 =( BOUNDED_CURVE ( )  B_SPLINE_CURVE ( 2, ( #20861, #3468, #21006, #11440, #995, #13157, #21121, #8976, #24919 ),
 .UNSPECIFIED., .F., .F. ) 
 B_SPLINE_CURVE_WITH_KNOTS ( ( 3, 2, 2, 2, 3 ),
 ( 0.1250000000000000000, 0.1333333333333333315, 0.1499999999999999944, 0.1666666666666666574, 0.1749999999999999889 ),
 .UNSPECIFIED. ) 
 CURVE ( )  GEOMETRIC_REPRESENTATION_ITEM ( )  RATIONAL_B_SPLINE_CURVE ( ( 0.9330127018922194093, 0.9330127018922194093, 1.000000000000000000, 0.8660254037844387076, 1.000000000000000000, 0.8660254037844387076, 1.000000000000000000, 0.9330127018922194093, 0.9330127018922194093 ) ) 
 REPRESENTATION_ITEM ( '' )  );
#22393 = EDGE_CURVE ( 'NONE', #9154, #12924, #16569, .T. ) ;
#22394 = ORIENTED_EDGE ( 'NONE', *, *, #19318, .T. ) ;
#22395 = VERTEX_POINT ( 'NONE', #2821 ) ;
#22396 = CARTESIAN_POINT ( 'NONE',  ( 8.012344526598182026E-15, 28.06562499938548783, 4.662447845253954171 ) ) ;
#22397 = ORIENTED_EDGE ( 'NONE', *, *, #25329, .F. ) ;
#22398 = DIRECTION ( 'NONE',  ( 0.000000000000000000, -0.000000000000000000, 1.000000000000000000 ) ) ;
#22399 = EDGE_LOOP ( 'NONE', ( #9760, #5592, #18769, #1026 ) ) ;
#22400 = DIRECTION ( 'NONE',  ( 0.000000000000000000, 0.000000000000000000, 1.000000000000000000 ) ) ;
#22401 = ADVANCED_FACE ( 'NONE', ( #18782 ), #18539, .F. ) ;
#22402 = EDGE_LOOP ( 'NONE', ( #1199, #11263, #8962 ) ) ;
#22403 = CARTESIAN_POINT ( 'NONE',  ( 26.25859848311259981, -16.66421332384692278, 1.000000000000000000 ) ) ;
#22404 = CARTESIAN_POINT ( 'NONE',  ( -1.071796769724484344, 25.97634618820330843, 4.999999999999992006 ) ) ;
#22405 = ORIENTED_EDGE ( 'NONE', *, *, #4843, .T. ) ;
#22406 = CARTESIAN_POINT ( 'NONE',  ( -0.1556054994193453167, 38.97851006807007224, 14.51964528620012551 ) ) ;
#22407 = CARTESIAN_POINT ( 'NONE',  ( 3.756430356250002323, 26.45312499938548356, 11.16877607737301226 ) ) ;
#22408 = LINE ( 'NONE', #20185, #22258 ) ;
#22409 = CARTESIAN_POINT ( 'NONE',  ( -14.54246377227319442, 27.49048467073874491, -6.500000000000000000 ) ) ;
#22410 = CARTESIAN_POINT ( 'NONE',  ( 0.000000000000000000, 0.000000000000000000, -6.500000000000000000 ) ) ;
#22411 = EDGE_CURVE ( 'NONE', #8734, #22340, #16839, .T. ) ;
#22412 = DIRECTION ( 'NONE',  ( 0.000000000000000000, 0.000000000000000000, 1.000000000000000000 ) ) ;
#22413 = CARTESIAN_POINT ( 'NONE',  ( 3.756430356250004099, 26.97812499938548569, 6.831223922626973533 ) ) ;
#22414 = EDGE_CURVE ( 'NONE', #15910, #23657, #11574, .T. ) ;
#22415 = CARTESIAN_POINT ( 'NONE',  ( 13.24173596767359662, -28.14012133169329388, -6.500000000000000000 ) ) ;
#22416 = FACE_OUTER_BOUND ( 'NONE', #2664, .T. ) ;
#22417 = EDGE_CURVE ( 'NONE', #7673, #17013, #15471, .T. ) ;
#22418 = FACE_OUTER_BOUND ( 'NONE', #20203, .T. ) ;
#22419 = DIRECTION ( 'NONE',  ( -0.000000000000000000, -0.000000000000000000, 1.000000000000000000 ) ) ;
#22420 = CARTESIAN_POINT ( 'NONE',  ( 3.756430356249996105, -26.22812499938548214, 6.831223922626973533 ) ) ;
#22421 = CARTESIAN_POINT ( 'NONE',  ( 2.000000000000000888, -12.46410161513774817, 0.3750000000000003331 ) ) ;
#22422 = EDGE_LOOP ( 'NONE', ( #4871, #17771, #14431, #25808 ) ) ;
#22423 = CARTESIAN_POINT ( 'NONE',  ( 3.756430356250002323, 26.11562499938548498, 11.16877607737301226 ) ) ;
#22424 = CARTESIAN_POINT ( 'NONE',  ( -2.620986760973688460E-15, -28.03750000000000142, 13.61880215351699874 ) ) ;
#22425 = EDGE_CURVE ( 'NONE', #9975, #5761, #9591, .T. ) ;
#22427 = ORIENTED_EDGE ( 'NONE', *, *, #576, .T. ) ;
#22426 = CARTESIAN_POINT ( 'NONE',  ( -3.756430356249997882, 28.62812499938548783, 8.999999999999992895 ) ) ;
#22428 = ORIENTED_EDGE ( 'NONE', *, *, #11237, .F. ) ;
#22429 =( BOUNDED_CURVE ( )  B_SPLINE_CURVE ( 2, ( #21979, #4322, #10318, #16102, #22239, #2361, #2105, #19874, #24066 ),
 .UNSPECIFIED., .F., .F. ) 
 B_SPLINE_CURVE_WITH_KNOTS ( ( 3, 2, 2, 2, 3 ),
 ( 0.9250000000000000444, 0.9333333333333333481, 0.9499999999999999556, 0.9666666666666666741, 0.9749999999999999778 ),
 .UNSPECIFIED. ) 
 CURVE ( )  GEOMETRIC_REPRESENTATION_ITEM ( )  RATIONAL_B_SPLINE_CURVE ( ( 0.9330127018922194093, 0.9330127018922198534, 1.000000000000000000, 0.8660254037844387076, 1.000000000000000000, 0.8660254037844387076, 1.000000000000000000, 0.9330127018922194093, 0.9330127018922194093 ) ) 
 REPRESENTATION_ITEM ( '' )  );
#22430 = CARTESIAN_POINT ( 'NONE',  ( -26.52310962334728828, 16.23990935651745460, -2.750000000000000000 ) ) ;
#22431 = EDGE_CURVE ( 'NONE', #25550, #2880, #8350, .T. ) ;
#22432 = CARTESIAN_POINT ( 'NONE',  ( 30.45149776762729488, 6.317933499823327637, -6.500000000000000000 ) ) ;
#22433 = CARTESIAN_POINT ( 'NONE',  ( -1.071796769724487230, 25.52634618820330559, 4.999999999999992006 ) ) ;
#22434 = VERTEX_POINT ( 'NONE', #23218 ) ;
#22435 = ORIENTED_EDGE ( 'NONE', *, *, #4394, .F. ) ;
#22436 = CARTESIAN_POINT ( 'NONE',  ( 3.756430356249997438, -27.76562499938549067, 11.16877607737301048 ) ) ;
#22437 = CARTESIAN_POINT ( 'NONE',  ( -1.878215178124998275, 26.79062499938548569, 12.25316411605951927 ) ) ;
#22438 =( BOUNDED_CURVE ( )  B_SPLINE_CURVE ( 2, ( #12949, #17389, #15423, #7436, #23395, #20788, #10842, #11105, #926 ),
 .UNSPECIFIED., .F., .F. ) 
 B_SPLINE_CURVE_WITH_KNOTS ( ( 3, 2, 2, 2, 3 ),
 ( 0.7750000000000000222, 0.7833333333333333259, 0.8000000000000000444, 0.8166666666666666519, 0.8250000000000000666 ),
 .UNSPECIFIED. ) 
 CURVE ( )  GEOMETRIC_REPRESENTATION_ITEM ( )  RATIONAL_B_SPLINE_CURVE ( ( 0.9330127018922194093, 0.9330127018922194093, 1.000000000000000000, 0.8660254037844387076, 1.000000000000000000, 0.8660254037844387076, 1.000000000000000000, 0.9330127018922189652, 0.9330127018922194093 ) ) 
 REPRESENTATION_ITEM ( '' )  );
#22439 = CARTESIAN_POINT ( 'NONE',  ( -30.53863125411922752, 1.952785157361987878, 1.000000000000000000 ) ) ;
#22440 = DIRECTION ( 'NONE',  ( 0.1873813145857330109, 0.9822872507286871668, 0.000000000000000000 ) ) ;
#22441 = CARTESIAN_POINT ( 'NONE',  ( -5.335677986744341794, 30.63887302793254364, -6.500000000000000000 ) ) ;
#22442 =( NAMED_UNIT ( * ) SI_UNIT ( $, .STERADIAN. ) SOLID_ANGLE_UNIT ( ) );
#22443 = CARTESIAN_POINT ( 'NONE',  ( -1.859271017917182139E-15, -28.48749999999999716, 12.99999999999999289 ) ) ;
#22444 = DIRECTION ( 'NONE',  ( 0.000000000000000000, 0.000000000000000000, 1.000000000000000000 ) ) ;
#22445 = AXIS2_PLACEMENT_3D ( 'NONE', #18105, #17573, #180 ) ;
#22446 = DIRECTION ( 'NONE',  ( 0.9921147013144794302, 0.1253332335642911299, 0.000000000000000000 ) ) ;
#22447 = CARTESIAN_POINT ( 'NONE',  ( -5.827558883616271501, -30.54913349766217934, 1.000000000000000000 ) ) ;
#22448 = CARTESIAN_POINT ( 'NONE',  ( 20.43103032403801578, 17.77483294607857189, 5.746835883940462963 ) ) ;
#22449 = CARTESIAN_POINT ( 'NONE',  ( 19.94483064597403299, 19.94483064597396194, 4.381197846482986158 ) ) ;
#22450 = DIRECTION ( 'NONE',  ( 0.000000000000000000, 1.000000000000000000, 0.000000000000000000 ) ) ;
#22451 = LINE ( 'NONE', #14749, #21360 ) ;
#22452 = CARTESIAN_POINT ( 'NONE',  ( 3.756430356250002323, 26.45312499938548356, 11.16877607737301226 ) ) ;
#22454 = ORIENTED_EDGE ( 'NONE', *, *, #5202, .T. ) ;
#22453 = CARTESIAN_POINT ( 'NONE',  ( -1.036406108997123487, 29.98318460927812268, 5.127803451112008304 ) ) ;
#22455 = CARTESIAN_POINT ( 'NONE',  ( 0.000000000000000000, 0.000000000000000000, -6.500000000000000000 ) ) ;
#22456 = CARTESIAN_POINT ( 'NONE',  ( 21.77888886054569539, 16.12203461105324820, 8.999999999999992895 ) ) ;
#22457 = ORIENTED_EDGE ( 'NONE', *, *, #14170, .T. ) ;
#22458 = CARTESIAN_POINT ( 'NONE',  ( 5.706339097771728319, 38.63519838069890966, 7.645898033751371337 ) ) ;
#22459 = LINE ( 'NONE', #127, #22784 ) ;
#22460 = CARTESIAN_POINT ( 'NONE',  ( 3.756430356249995661, -26.67812499938548498, 6.831223922626973533 ) ) ;
#22461 = EDGE_CURVE ( 'NONE', #4270, #5730, #10593, .T. ) ;
#22463 = ORIENTED_EDGE ( 'NONE', *, *, #25163, .T. ) ;
#22462 = DIRECTION ( 'NONE',  ( 0.000000000000000000, 0.000000000000000000, 1.000000000000000000 ) ) ;
#22464 = CARTESIAN_POINT ( 'NONE',  ( 15.92316082797555055, 21.58001507746786274, 8.999999999999992895 ) ) ;
#22465 = EDGE_CURVE ( 'NONE', #16533, #12207, #13268, .T. ) ;
#22466 = ORIENTED_EDGE ( 'NONE', *, *, #14614, .T. ) ;
#22467 = CARTESIAN_POINT ( 'NONE',  ( 3.756430356249995661, -26.22812499938548214, 6.831223922626973533 ) ) ;
#22468 = ORIENTED_EDGE ( 'NONE', *, *, #22094, .F. ) ;
#22469 = ORIENTED_EDGE ( 'NONE', *, *, #2307, .T. ) ;
#22470 = PRESENTATION_STYLE_ASSIGNMENT (( #14769 ) ) ;
#22471 = EDGE_CURVE ( 'NONE', #24696, #4508, #22840, .T. ) ;
#22472 = CARTESIAN_POINT ( 'NONE',  ( 1.878215178125003382, 25.32812499938548356, 5.746835883940462963 ) ) ;
#22473 = EDGE_CURVE ( 'NONE', #3500, #21315, #15038, .T. ) ;
#22474 = VECTOR ( 'NONE', #23426, 1000.000000000000000 ) ;
#22475 = CARTESIAN_POINT ( 'NONE',  ( -0.5000000000000000000, -0.8660254037844387076, 20.00000000000000000 ) ) ;
#22476 = VECTOR ( 'NONE', #21468, 1000.000000000000000 ) ;
#22477 = CARTESIAN_POINT ( 'NONE',  ( -3.756430356249997882, -11.16877607737301226, 0.9656249993854834068 ) ) ;
#22478 = CARTESIAN_POINT ( 'NONE',  ( 21.05852382634284936, 21.05852382634277831, 12.99999999999999289 ) ) ;
#22479 = CARTESIAN_POINT ( 'NONE',  ( 3.756430356250004099, 25.62812499938548072, 6.831223922626973533 ) ) ;
#22480 = CARTESIAN_POINT ( 'NONE',  ( 18.38477631085027753, 21.21320343559639454, 12.46410161513774639 ) ) ;
#22481 = CARTESIAN_POINT ( 'NONE',  ( 4.000000000000018652, -6.690598923241496188, 3.637499999999998401 ) ) ;
#22482 = CARTESIAN_POINT ( 'NONE',  ( -3.756430356249997438, 25.85312499938548569, 11.16877607737301048 ) ) ;
#22483 = DIRECTION ( 'NONE',  ( 0.000000000000000000, -0.000000000000000000, 1.000000000000000000 ) ) ;
#22484 = CYLINDRICAL_SURFACE ( 'NONE', #2441, 31.10000000000000142 ) ;
#22485 = CARTESIAN_POINT ( 'NONE',  ( -0.7500000000000001110, 20.00000000000000000, 17.69999999999999929 ) ) ;
#22486 = CARTESIAN_POINT ( 'NONE',  ( -3.756430356250003655, -27.95312499938548711, 8.999999999999992895 ) ) ;
#22487 = CARTESIAN_POINT ( 'NONE',  ( 0.000000000000000000, 0.000000000000000000, 19.50000000000000000 ) ) ;
#22488 = CARTESIAN_POINT ( 'NONE',  ( -1.999999999999995781, -5.535898384862237620, 2.849999999999998312 ) ) ;
#22489 = AXIS2_PLACEMENT_3D ( 'NONE', #6116, #8338, #16327 ) ;
#22490 = LINE ( 'NONE', #9021, #23347 ) ;
#22491 = DIRECTION ( 'NONE',  ( 0.000000000000000000, 0.000000000000000000, 1.000000000000000000 ) ) ;
#22492 = ORIENTED_EDGE ( 'NONE', *, *, #23531, .F. ) ;
#22493 = DIRECTION ( 'NONE',  ( -0.1873813145857119722, 0.9822872507286911636, 0.000000000000000000 ) ) ;
#22495 = ORIENTED_EDGE ( 'NONE', *, *, #24165, .F. ) ;
#22494 = DIRECTION ( 'NONE',  ( -0.000000000000000000, -0.000000000000000000, 1.000000000000000000 ) ) ;
#22497 = ADVANCED_FACE ( 'NONE', ( #10928 ), #7142, .F. ) ;
#22496 = CIRCLE ( 'NONE', #10423, 0.5000000000000001110 ) ;
#22498 = ORIENTED_EDGE ( 'NONE', *, *, #23220, .F. ) ;
#22500 = VERTEX_POINT ( 'NONE', #13035 ) ;
#22499 = VECTOR ( 'NONE', #19336, 1000.000000000000000 ) ;
#22501 = ORIENTED_EDGE ( 'NONE', *, *, #9867, .T. ) ;
#22502 = EDGE_LOOP ( 'NONE', ( #19242, #24307, #20495, #7930, #2720 ) ) ;
#22503 = VERTEX_POINT ( 'NONE', #11808 ) ;
#22504 = CYLINDRICAL_SURFACE ( 'NONE', #25165, 4.000000000000000000 ) ;
#22505 = ORIENTED_EDGE ( 'NONE', *, *, #7737, .T. ) ;
#22506 = DIRECTION ( 'NONE',  ( 1.000000000000000000, 0.000000000000000000, 0.000000000000000000 ) ) ;
#22507 = CARTESIAN_POINT ( 'NONE',  ( 3.756430356250003211, 28.44062499938548427, 6.831223922626973533 ) ) ;
#22508 = EDGE_CURVE ( 'NONE', #12276, #17574, #10874, .T. ) ;
#22509 = AXIS2_PLACEMENT_3D ( 'NONE', #19169, #7154, #25067 ) ;
#22510 = ADVANCED_BREP_SHAPE_REPRESENTATION ( '', ( #22659, #21036 ), #8945 ) ;
#22511 = CARTESIAN_POINT ( 'NONE',  ( 3.756430356250004099, -6.831223922626973533, 2.990624999385484539 ) ) ;
#22512 = CIRCLE ( 'NONE', #2826, 31.10000000000000142 ) ;
#22513 = CARTESIAN_POINT ( 'NONE',  ( -3.897863563850083146, -30.85476721088024021, 1.000000000000000000 ) ) ;
#22514 = CARTESIAN_POINT ( 'NONE',  ( 15.57168961538060969, 20.88408437129928785, 6.831223922626973533 ) ) ;
#22515 = SHAPE_REPRESENTATION ( 'bezel locker', ( #21036 ), #21481 ) ;
#22516 = CYLINDRICAL_SURFACE ( 'NONE', #41, 0.7500000000000001110 ) ;
#22517 = AXIS2_PLACEMENT_3D ( 'NONE', #9356, #7381, #10913 ) ;
#22518 = DIRECTION ( 'NONE',  ( 1.000000000000000000, 0.000000000000000000, 0.000000000000000000 ) ) ;
#22519 = CIRCLE ( 'NONE', #12928, 0.5000000000000005551 ) ;
#22520 = CARTESIAN_POINT ( 'NONE',  ( 3.756430356250003655, -8.999999999999992895, 2.840624999385484184 ) ) ;
#22521 = FILL_AREA_STYLE_COLOUR ( '', #6651 ) ;
#22522 = CARTESIAN_POINT ( 'NONE',  ( 4.000000000000003553, -6.690598923241489970, 4.087499999999997691 ) ) ;
#22523 = CARTESIAN_POINT ( 'NONE',  ( 1.394453263437886604E-15, 28.88124999877097210, 12.99999999999999289 ) ) ;
#22524 = LINE ( 'NONE', #12195, #18860 ) ;
#22525 = CARTESIAN_POINT ( 'NONE',  ( 2.672651547586948120E-15, -13.33755215474603162, 1.940624999385484939 ) ) ;
#22526 = CARTESIAN_POINT ( 'NONE',  ( 4.000000000000003553, 27.64374999877096784, 8.999999999999992895 ) ) ;
#22527 = VERTEX_POINT ( 'NONE', #9234 ) ;
#22528 = EDGE_LOOP ( 'NONE', ( #6219, #3945, #23298, #13957 ) ) ;
#22529 = CARTESIAN_POINT ( 'NONE',  ( -3.756430356249994773, 28.17812499938548854, 8.999999999999992895 ) ) ;
#22531 = ORIENTED_EDGE ( 'NONE', *, *, #846, .T. ) ;
#22530 = CIRCLE ( 'NONE', #13755, 0.4999999999999996114 ) ;
#22532 = LINE ( 'NONE', #6181, #19545 ) ;
#22533 = ORIENTED_EDGE ( 'NONE', *, *, #17300, .T. ) ;
#22534 = CARTESIAN_POINT ( 'NONE',  ( -1.999999999999995781, -5.535898384862237620, 2.343749998770968013 ) ) ;
#22535 = ORIENTED_EDGE ( 'NONE', *, *, #17469, .F. ) ;
#22536 = FACE_BOUND ( 'NONE', #13856, .T. ) ;
#22537 = AXIS2_PLACEMENT_3D ( 'NONE', #20440, #17982, #72 ) ;
#22538 = CARTESIAN_POINT ( 'NONE',  ( -3.999999999999997335, 29.25624999877096855, 11.30940107675849404 ) ) ;
#22539 = AXIS2_PLACEMENT_3D ( 'NONE', #11576, #9627, #3607 ) ;
#22540 = ORIENTED_EDGE ( 'NONE', *, *, #5662, .T. ) ;
#22541 = ADVANCED_FACE ( 'NONE', ( #3336 ), #9841, .F. ) ;
#22542 = FACE_OUTER_BOUND ( 'NONE', #18647, .T. ) ;
#22543 = CARTESIAN_POINT ( 'NONE',  ( 2.672651547586948120E-15, 29.52812499938548285, 13.33755215474602984 ) ) ;
#22544 = CARTESIAN_POINT ( 'NONE',  ( 1.859271017917182139E-15, 28.93749999999999645, 12.99999999999999289 ) ) ;
#22545 = VECTOR ( 'NONE', #8909, 1000.000000000000000 ) ;
#22546 = LINE ( 'NONE', #10507, #7570 ) ;
#22547 = CARTESIAN_POINT ( 'NONE',  ( -3.999999999999995559, 28.28124999877096712, 6.690598923241487306 ) ) ;
#22548 = CARTESIAN_POINT ( 'NONE',  ( -1.999999999999994893, 28.75000000000000355, 5.535898384862237620 ) ) ;
#22549 = EDGE_CURVE ( 'NONE', #17200, #23624, #11669, .T. ) ;
#22550 = AXIS2_PLACEMENT_3D ( 'NONE', #21134, #25313, #7143 ) ;
#22551 = AXIS2_PLACEMENT_3D ( 'NONE', #1656, #21530, #9497 ) ;
#22552 =( BOUNDED_CURVE ( )  B_SPLINE_CURVE ( 2, ( #12678, #2730, #10694, #18681, #8618, #16597, #24701, #767, #12404 ),
 .UNSPECIFIED., .F., .F. ) 
 B_SPLINE_CURVE_WITH_KNOTS ( ( 3, 2, 2, 2, 3 ),
 ( 0.5750000000000000666, 0.5833333333333333703, 0.5999999999999999778, 0.6166666666666666963, 0.6250000000000000000 ),
 .UNSPECIFIED. ) 
 CURVE ( )  GEOMETRIC_REPRESENTATION_ITEM ( )  RATIONAL_B_SPLINE_CURVE ( ( 0.9330127018922194093, 0.9330127018922198534, 1.000000000000000000, 0.8660254037844387076, 1.000000000000000000, 0.8660254037844387076, 1.000000000000000000, 0.9330127018922194093, 0.9330127018922194093 ) ) 
 REPRESENTATION_ITEM ( '' )  );
#22553 = CARTESIAN_POINT ( 'NONE',  ( 2.672651547586948120E-15, 27.27812499938548285, 13.33755215474602984 ) ) ;
#22554 = AXIS2_PLACEMENT_3D ( 'NONE', #10787, #14476, #16452 ) ;
#22555 = CARTESIAN_POINT ( 'NONE',  ( 20.85756786700484966, 15.54517311108603295, 6.831223922626973533 ) ) ;
#22556 = CARTESIAN_POINT ( 'NONE',  ( 2.000000000000000888, -12.46410161513774817, 2.174999999999999822 ) ) ;
#22557 = CARTESIAN_POINT ( 'NONE',  ( -1.057460391440397258E-14, 29.16249999999999787, 4.999999999999992006 ) ) ;
#22558 = CARTESIAN_POINT ( 'NONE',  ( 3.999999999999996447, -27.86874999877096570, 8.999999999999992895 ) ) ;
#22559 = CARTESIAN_POINT ( 'NONE',  ( 3.756430356249996994, -26.71562499938548285, 8.999999999999992895 ) ) ;
#22560 = CARTESIAN_POINT ( 'NONE',  ( 5.732828587490932826, 38.61000136877622424, 10.35167381828165567 ) ) ;
#22561 = AXIS2_PLACEMENT_3D ( 'NONE', #335, #16295, #11296 ) ;
#22562 = B_SPLINE_CURVE_WITH_KNOTS ( 'NONE', 3,
 ( #6196, #10243, #10127, #18240, #6335, #4370, #14328, #4492 ),
 .UNSPECIFIED., .F., .F.,
 ( 4, 2, 2, 4 ),
 ( 0.01599790909976502723, 0.01669365098321972177, 0.01738939286667441630, 0.01878087663358380885 ),
 .UNSPECIFIED. ) ;
#22563 = VERTEX_POINT ( 'NONE', #17823 ) ;
#22564 = CARTESIAN_POINT ( 'NONE',  ( -3.999999999999996447, 29.21874999877096712, 8.999999999999992895 ) ) ;
#22565 = ADVANCED_FACE ( 'NONE', ( #17223 ), #15736, .F. ) ;
#22566 = CARTESIAN_POINT ( 'NONE',  ( 3.999999999999997335, -29.31250000000000000, 11.30940107675849404 ) ) ;
#22568 = ORIENTED_EDGE ( 'NONE', *, *, #7623, .T. ) ;
#22567 = FACE_OUTER_BOUND ( 'NONE', #23818, .T. ) ;
#22569 = ORIENTED_EDGE ( 'NONE', *, *, #15047, .F. ) ;
#22570 = LINE ( 'NONE', #8313, #11232 ) ;
#22571 = AXIS2_PLACEMENT_3D ( 'NONE', #13253, #977, #22935 ) ;
#22572 = ADVANCED_FACE ( 'NONE', ( #19647 ), #23699, .T. ) ;
#22573 = DIRECTION ( 'NONE',  ( 0.000000000000000000, 0.000000000000000000, 1.000000000000000000 ) ) ;
#22574 = VERTEX_POINT ( 'NONE', #19783 ) ;
#22575 = CARTESIAN_POINT ( 'NONE',  ( -3.756430356250003211, -27.09062499938548640, 6.831223922626973533 ) ) ;
#22576 = CARTESIAN_POINT ( 'NONE',  ( -3.756430356249994773, 27.16562499938548214, 8.999999999999992895 ) ) ;
#22577 = CARTESIAN_POINT ( 'NONE',  ( 20.59006558380675855, 17.76163845906049943, 12.46410161513774817 ) ) ;
#22578 = CIRCLE ( 'NONE', #5025, 0.5000000000000000000 ) ;
#22579 = EDGE_CURVE ( 'NONE', #19382, #25812, #25790, .T. ) ;
#22580 = CARTESIAN_POINT ( 'NONE',  ( -1.878215178124998275, 27.24062499938548854, 12.25316411605951927 ) ) ;
#22581 = EDGE_CURVE ( 'NONE', #22072, #14590, #2962, .T. ) ;
#22582 = CIRCLE ( 'NONE', #20061, 6.000000000000000000 ) ;
#22583 = CARTESIAN_POINT ( 'NONE',  ( 4.000000000000003553, -8.999999999999992895, 0.9000000000000014655 ) ) ;
#22584 = CARTESIAN_POINT ( 'NONE',  ( 0.000000000000000000, -25.00000000000000000, 0.000000000000000000 ) ) ;
#22585 = ADVANCED_FACE ( 'NONE', ( #10095 ), #4075, .T. ) ;
#22586 = CARTESIAN_POINT ( 'NONE',  ( 3.469446951953614189E-15, 40.00000000000000000, 8.999999999999992895 ) ) ;
#22587 = CARTESIAN_POINT ( 'NONE',  ( -29.41953157733080104, 10.08469938919530406, -6.500000000000000000 ) ) ;
#22588 = CARTESIAN_POINT ( 'NONE',  ( 3.999999999999997335, -28.35624999877096997, 11.30940107675849404 ) ) ;
#22589 = CARTESIAN_POINT ( 'NONE',  ( 16.55280027427694378, 21.86519503019561839, 8.999999999999992895 ) ) ;
#22590 = CARTESIAN_POINT ( 'NONE',  ( 20.58122674904193516, 20.58122674904185345, 4.381197846482986158 ) ) ;
#22591 = AXIS2_PLACEMENT_3D ( 'NONE', #23889, #5971, #13954 ) ;
#22592 = DIRECTION ( 'NONE',  ( -0.000000000000000000, -1.000000000000000000, -0.000000000000000000 ) ) ;
#22593 = CARTESIAN_POINT ( 'NONE',  ( -0.4995657836784015426, 38.49999999999999289, 3.020833333333323267 ) ) ;
#22594 = CARTESIAN_POINT ( 'NONE',  ( 3.735045420075836212E-15, 28.96562499938548640, 4.662447845253954171 ) ) ;
#22595 = AXIS2_PLACEMENT_3D ( 'NONE', #10062, #6272, #23934 ) ;
#22597 = ORIENTED_EDGE ( 'NONE', *, *, #10109, .F. ) ;
#22596 = LINE ( 'NONE', #19046, #21252 ) ;
#22598 = PLANE ( 'NONE',  #2057 ) ;
#22599 = DIRECTION ( 'NONE',  ( -0.000000000000000000, -0.000000000000000000, 1.000000000000000000 ) ) ;
#22600 = ORIENTED_EDGE ( 'NONE', *, *, #25661, .T. ) ;
#22601 = CARTESIAN_POINT ( 'NONE',  ( 11.91206721063030649, -28.72825533807137433, -2.750000000000000000 ) ) ;
#22602 = CARTESIAN_POINT ( 'NONE',  ( 2.000000000000003997, 28.61874999877096926, 5.535898384862238508 ) ) ;
#22603 = CARTESIAN_POINT ( 'NONE',  ( 3.756430356249997882, -25.85312499938548925, 11.16877607737301226 ) ) ;
#22605 = VERTEX_POINT ( 'NONE', #22000 ) ;
#22604 = DIRECTION ( 'NONE',  ( 0.000000000000000000, 0.000000000000000000, 1.000000000000000000 ) ) ;
#22606 =( BOUNDED_CURVE ( )  B_SPLINE_CURVE ( 2, ( #18324, #23958, #22111, #4066, #16235, #10084, #21868, #14287, #2252 ),
 .UNSPECIFIED., .F., .T. ) 
 B_SPLINE_CURVE_WITH_KNOTS ( ( 3, 2, 2, 2, 3 ),
 ( 0.6750000000000000444, 0.6833333333333333481, 0.6999999999999999556, 0.7166666666666666741, 0.7249999999999999778 ),
 .UNSPECIFIED. ) 
 CURVE ( )  GEOMETRIC_REPRESENTATION_ITEM ( )  RATIONAL_B_SPLINE_CURVE ( ( 0.9330127018922194093, 0.9330127018922198534, 1.000000000000000000, 0.8660254037844387076, 1.000000000000000000, 0.8660254037844387076, 1.000000000000000000, 0.9330127018922194093, 0.9330127018922194093 ) ) 
 REPRESENTATION_ITEM ( '' )  );
#22607 = AXIS2_PLACEMENT_3D ( 'NONE', #11445, #8980, #5048 ) ;
#22608 = ORIENTED_EDGE ( 'NONE', *, *, #21964, .F. ) ;
#22609 = CARTESIAN_POINT ( 'NONE',  ( -3.756430356250004099, -26.52812499938548285, 6.831223922626973533 ) ) ;
#22610 = ORIENTED_EDGE ( 'NONE', *, *, #19449, .T. ) ;
#22611 = ORIENTED_EDGE ( 'NONE', *, *, #7684, .F. ) ;
#22612 = CARTESIAN_POINT ( 'NONE',  ( -16.66421332384701515, -26.25859848311253941, -6.500000000000000000 ) ) ;
#22613 = CARTESIAN_POINT ( 'NONE',  ( 8.012344526598182026E-15, 25.81562499938549138, 4.662447845253954171 ) ) ;
#22614 = PRODUCT_RELATED_PRODUCT_CATEGORY ( 'part', '', ( #22379 ) ) ;
#22615 = CARTESIAN_POINT ( 'NONE',  ( -1.999999999999998224, -12.46410161513774639, 3.393749998770966503 ) ) ;
#22616 = AXIS2_PLACEMENT_3D ( 'NONE', #17228, #15254, #11955 ) ;
#22617 = CARTESIAN_POINT ( 'NONE',  ( 2.672651547586948120E-15, -13.33755215474602984, 2.390624999385484450 ) ) ;
#22618 = FILL_AREA_STYLE_COLOUR ( '', #22277 ) ;
#22619 = EDGE_CURVE ( 'NONE', #2418, #16864, #22578, .T. ) ;
#22620 = FACE_OUTER_BOUND ( 'NONE', #25292, .T. ) ;
#22621 = CARTESIAN_POINT ( 'NONE',  ( 3.756430356250003655, 28.29062499938548569, 8.999999999999992895 ) ) ;
#22622 = EDGE_CURVE ( 'NONE', #14319, #18045, #175, .T. ) ;
#22623 = CARTESIAN_POINT ( 'NONE',  ( 23.34336261392093093, 17.68650836442847663, 11.30940107675849760 ) ) ;
#22624 = AXIS2_PLACEMENT_3D ( 'NONE', #25540, #13520, #2125 ) ;
#22625 = DIRECTION ( 'NONE',  ( 1.000000000000000000, 0.000000000000000000, 0.000000000000000000 ) ) ;
#22626 = CARTESIAN_POINT ( 'NONE',  ( -3.756430356249996105, 28.92812499938548498, 6.831223922626973533 ) ) ;
#22627 = DIRECTION ( 'NONE',  ( -0.000000000000000000, -0.000000000000000000, -1.000000000000000000 ) ) ;
#22628 = CARTESIAN_POINT ( 'NONE',  ( 0.5000000000000000000, -2.999999999999999556, 19.50000000000000000 ) ) ;
#22629 = CARTESIAN_POINT ( 'NONE',  ( 22.67092431280578779, -21.28941499438234786, 1.000000000000000000 ) ) ;
#22630 = CARTESIAN_POINT ( 'NONE',  ( 1.878215178124998497, -26.00312499938548783, 12.25316411605951927 ) ) ;
#22631 = AXIS2_PLACEMENT_3D ( 'NONE', #7526, #15522, #23490 ) ;
#22632 = CARTESIAN_POINT ( 'NONE',  ( 3.756430356250002323, 29.71562499938548640, 11.16877607737301226 ) ) ;
#22633 = AXIS2_PLACEMENT_3D ( 'NONE', #23047, #7463, #15203 ) ;
#22634 = DIRECTION ( 'NONE',  ( -0.000000000000000000, -1.000000000000000000, 0.000000000000000000 ) ) ;
#22635 = DIRECTION ( 'NONE',  ( 1.000000000000000000, 0.000000000000000000, 0.000000000000000000 ) ) ;
#22636 = CARTESIAN_POINT ( 'NONE',  ( -25.99307600111999150, 0.5999999999999998668, 19.59999999999999787 ) ) ;
#22637 = VERTEX_POINT ( 'NONE', #15861 ) ;
#22638 = CARTESIAN_POINT ( 'NONE',  ( -2.451530025008687996, 31.00322564728517349, 1.000000000000000000 ) ) ;
#22640 = VERTEX_POINT ( 'NONE', #1994 ) ;
#22639 = LINE ( 'NONE', #6540, #19990 ) ;
#22641 = CIRCLE ( 'NONE', #9678, 0.4999999999999996669 ) ;
#22642 = ORIENTED_EDGE ( 'NONE', *, *, #2161, .T. ) ;
#22643 = ORIENTED_EDGE ( 'NONE', *, *, #21773, .F. ) ;
#22644 = ORIENTED_EDGE ( 'NONE', *, *, #8813, .T. ) ;
#22645 = ORIENTED_EDGE ( 'NONE', *, *, #2992, .T. ) ;
#22646 = CARTESIAN_POINT ( 'NONE',  ( -17.08421000182795879, -25.98730014090424234, -2.750000000000000000 ) ) ;
#22647 = ORIENTED_EDGE ( 'NONE', *, *, #4922, .F. ) ;
#22648 = DIRECTION ( 'NONE',  ( 1.000000000000000000, 0.000000000000000000, 0.000000000000000000 ) ) ;
#22649 = CARTESIAN_POINT ( 'NONE',  ( -3.756430356249996994, 28.17812499938548498, 8.999999999999992895 ) ) ;
#22650 = AXIS2_PLACEMENT_3D ( 'NONE', #15289, #15173, #14906 ) ;
#22651 = ADVANCED_FACE ( 'NONE', ( #12191 ), #8146, .F. ) ;
#22652 = CARTESIAN_POINT ( 'NONE',  ( -3.756430356249996994, -8.999999999999992895, 2.278124999385483740 ) ) ;
#22653 = LINE ( 'NONE', #6824, #6679 ) ;
#22654 = DIRECTION ( 'NONE',  ( -0.000000000000000000, -0.000000000000000000, -1.000000000000000000 ) ) ;
#22655 = AXIS2_PLACEMENT_3D ( 'NONE', #2429, #24017, #24525 ) ;
#22656 = DIRECTION ( 'NONE',  ( -1.000000000000000000, 0.000000000000000000, 0.000000000000000000 ) ) ;
#22657 = ADVANCED_FACE ( 'NONE', ( #8017, #8403 ), #6049, .T. ) ;
#22658 = CARTESIAN_POINT ( 'NONE',  ( 26.00000000000000711, -1.701696020694468015, 20.00001200000000168 ) ) ;
#22659 = MANIFOLD_SOLID_BREP ( 'Cavity1', #24656 ) ;
#22660 = CARTESIAN_POINT ( 'NONE',  ( 1.878215178125004048, -5.746835883940462963, 3.815624999385484273 ) ) ;
#22661 = DIRECTION ( 'NONE',  ( 1.000000000000000000, 0.000000000000000000, 0.000000000000000000 ) ) ;
#22662 = CARTESIAN_POINT ( 'NONE',  ( -3.999999999999996447, 27.86874999877096570, 8.999999999999992895 ) ) ;
#22663 = CARTESIAN_POINT ( 'NONE',  ( 0.000000000000000000, 0.000000000000000000, 19.00000000000000000 ) ) ;
#22664 = DIRECTION ( 'NONE',  ( 0.000000000000000000, 0.000000000000000000, 1.000000000000000000 ) ) ;
#22665 = CARTESIAN_POINT ( 'NONE',  ( 3.735045420075836212E-15, -4.662447845253954171, 0.8156249993854834957 ) ) ;
#22666 = CARTESIAN_POINT ( 'NONE',  ( 0.000000000000000000, 0.000000000000000000, -6.500000000000000000 ) ) ;
#22667 = CIRCLE ( 'NONE', #8886, 0.4999999999999992784 ) ;
#22668 = CARTESIAN_POINT ( 'NONE',  ( 0.000000000000000000, 0.000000000000000000, 1.000000000000000000 ) ) ;
#22669 = ORIENTED_EDGE ( 'NONE', *, *, #2160, .F. ) ;
#22670 = ADVANCED_FACE ( 'NONE', ( #2263 ), #23833, .F. ) ;
#22671 = ORIENTED_EDGE ( 'NONE', *, *, #3970, .F. ) ;
#22672 = CARTESIAN_POINT ( 'NONE',  ( 4.006172263299091013E-15, 28.96562499938548996, 4.662447845253954171 ) ) ;
#22673 = AXIS2_PLACEMENT_3D ( 'NONE', #10250, #8661, #8795 ) ;
#22674 = EDGE_CURVE ( 'NONE', #7996, #24829, #25078, .T. ) ;
#22675 = ORIENTED_EDGE ( 'NONE', *, *, #16969, .T. ) ;
#22676 = CARTESIAN_POINT ( 'NONE',  ( 3.369928719974892281E-15, 25.11250000000000426, 4.999999999999992006 ) ) ;
#22677 = ORIENTED_EDGE ( 'NONE', *, *, #23832, .F. ) ;
#22678 = CARTESIAN_POINT ( 'NONE',  ( -3.756430356250004099, -25.74062499938548143, 6.831223922626973533 ) ) ;
#22679 = EDGE_LOOP ( 'NONE', ( #444, #309, #20181, #21000 ) ) ;
#22680 = DIRECTION ( 'NONE',  ( 1.000000000000000000, 0.000000000000000000, -0.000000000000000000 ) ) ;
#22681 = VERTEX_POINT ( 'NONE', #22265 ) ;
#22682 = FACE_OUTER_BOUND ( 'NONE', #22825, .T. ) ;
#22683 = CARTESIAN_POINT ( 'NONE',  ( 2.620986760973688460E-15, 25.78750000000000142, 13.61880215351699874 ) ) ;
#22684 = CARTESIAN_POINT ( 'NONE',  ( 16.25461713252580509, 21.91147138201811373, 6.690598923241487306 ) ) ;
#22685 = CARTESIAN_POINT ( 'NONE',  ( 0.000000000000000000, 0.000000000000000000, -6.500000000000000000 ) ) ;
#22686 = CYLINDRICAL_SURFACE ( 'NONE', #8322, 31.10000000000000142 ) ;
#22687 = CARTESIAN_POINT ( 'NONE',  ( 20.83105136271035462, 15.51865660679153969, 8.999999999999992895 ) ) ;
#22688 = EDGE_CURVE ( 'NONE', #585, #6457, #19634, .T. ) ;
#22689 = AXIS2_PLACEMENT_3D ( 'NONE', #1827, #9791, #1946 ) ;
#22690 = CARTESIAN_POINT ( 'NONE',  ( -3.756430356249996994, 27.16562499938548214, 8.999999999999992895 ) ) ;
#22691 = EDGE_CURVE ( 'NONE', #990, #12604, #20287, .T. ) ;
#22692 = CARTESIAN_POINT ( 'NONE',  ( -0.5000000000000000000, 0.000000000000000000, 19.50000000000000000 ) ) ;
#22693 = CARTESIAN_POINT ( 'NONE',  ( 19.74153744638290320, 16.91311032163664407, 5.535898384862238508 ) ) ;
#22694 = AXIS2_PLACEMENT_3D ( 'NONE', #18127, #464, #16543 ) ;
#22695 = CARTESIAN_POINT ( 'NONE',  ( 21.21320343559646915, 21.21320343559638744, 4.999999999999992006 ) ) ;
#22696 = DIRECTION ( 'NONE',  ( -0.000000000000000000, -0.000000000000000000, -1.000000000000000000 ) ) ;
#22697 = CYLINDRICAL_SURFACE ( 'NONE', #14183, 0.5000000000000002220 ) ;
#22698 = CARTESIAN_POINT ( 'NONE',  ( 3.756430356249996994, -27.16562499938548214, 8.999999999999992895 ) ) ;
#22699 = ADVANCED_FACE ( 'NONE', ( #4465 ), #20408, .T. ) ;
#22700 = DIRECTION ( 'NONE',  ( 1.000000000000000000, 0.000000000000000000, 0.000000000000000000 ) ) ;
#22701 = EDGE_LOOP ( 'NONE', ( #12425, #20458, #23592, #21508 ) ) ;
#22702 = CARTESIAN_POINT ( 'NONE',  ( -1.878215178124998497, 26.45312499938548711, 12.25316411605951927 ) ) ;
#22703 = CARTESIAN_POINT ( 'NONE',  ( 1.427366165835751044, 29.96717973704832261, 12.74788474329069921 ) ) ;
#22705 = VERTEX_POINT ( 'NONE', #5129 ) ;
#22704 = CARTESIAN_POINT ( 'NONE',  ( -1.878215178124999829, 29.15312499938549351, 12.25316411605951927 ) ) ;
#22706 = VERTEX_POINT ( 'NONE', #14810 ) ;
#22707 = CARTESIAN_POINT ( 'NONE',  ( -1.071796769724488563, 28.86115380933863506, 12.99999999999999289 ) ) ;
#22708 = CARTESIAN_POINT ( 'NONE',  ( -1.999999999999998224, -12.46410161513774639, 4.293749998770968190 ) ) ;
#22709 = ORIENTED_EDGE ( 'NONE', *, *, #3230, .F. ) ;
#22710 = CARTESIAN_POINT ( 'NONE',  ( -3.756430356250002323, -27.01562499938548356, 11.16877607737301403 ) ) ;
#22711 = CARTESIAN_POINT ( 'NONE',  ( -3.756430356249996105, 29.37812499938548427, 6.831223922626973533 ) ) ;
#22712 = CARTESIAN_POINT ( 'NONE',  ( 3.756430356250002323, 26.52812499938548640, 6.831223922626973533 ) ) ;
#22713 =( GEOMETRIC_REPRESENTATION_CONTEXT ( 3 ) GLOBAL_UNCERTAINTY_ASSIGNED_CONTEXT ( ( #10700 ) ) GLOBAL_UNIT_ASSIGNED_CONTEXT ( ( #1847, #13727, #7839 ) ) REPRESENTATION_CONTEXT ( 'NONE', 'WORKASPACE' ) );
#22714 = CARTESIAN_POINT ( 'NONE',  ( 5.112995299272250684E-15, 25.56250000000000711, 4.999999999999992006 ) ) ;
#22715 = CARTESIAN_POINT ( 'NONE',  ( -1.878215178124994722, 26.64062499938549067, 5.746835883940462963 ) ) ;
#22716 = AXIS2_PLACEMENT_3D ( 'NONE', #11025, #6972, #4882 ) ;
#22717 = CARTESIAN_POINT ( 'NONE',  ( -9.610428525060479288, 29.57785765677940404, 1.000000000000000000 ) ) ;
#22718 = CARTESIAN_POINT ( 'NONE',  ( 3.999999999999954259, -6.690598923241460660, 0.9375000000000014433 ) ) ;
#22719 = DIRECTION ( 'NONE',  ( 0.000000000000000000, 0.000000000000000000, 1.000000000000000000 ) ) ;
#22720 = DIRECTION ( 'NONE',  ( 0.000000000000000000, 1.000000000000000000, 0.000000000000000000 ) ) ;
#22721 = EDGE_CURVE ( 'NONE', #21735, #18967, #25530, .T. ) ;
#22722 = DIRECTION ( 'NONE',  ( 1.000000000000000000, 0.000000000000000000, 0.000000000000000000 ) ) ;
#22723 = CARTESIAN_POINT ( 'NONE',  ( 3.999999999999995559, -28.28124999877096712, 6.690598923241487306 ) ) ;
#22724 = CARTESIAN_POINT ( 'NONE',  ( 20.64316235839397962, 17.98696498043453573, 12.25316411605952283 ) ) ;
#22725 = CARTESIAN_POINT ( 'NONE',  ( 16.02247018838703241, 21.33486494430570701, 11.16877607737301226 ) ) ;
#22726 = CARTESIAN_POINT ( 'NONE',  ( 3.369928719974892281E-15, 25.50624999877096855, 4.999999999999992006 ) ) ;
#22727 = DIRECTION ( 'NONE',  ( 0.2588190451025209615, -0.9659258262890682012, 0.000000000000000000 ) ) ;
#22728 = CARTESIAN_POINT ( 'NONE',  ( 2.672651547586948120E-15, 27.72812499938548569, 13.33755215474602984 ) ) ;
#22730 = EDGE_CURVE ( 'NONE', #8768, #19772, #4747, .T. ) ;
#22729 = CARTESIAN_POINT ( 'NONE',  ( 27.92360179968377309, 13.69242354489143665, -6.500000000000000000 ) ) ;
#22731 = CARTESIAN_POINT ( 'NONE',  ( 21.06969990136081705, 15.75730514544200211, 8.999999999999992895 ) ) ;
#22732 = FACE_OUTER_BOUND ( 'NONE', #19061, .T. ) ;
#22733 = ORIENTED_EDGE ( 'NONE', *, *, #8784, .F. ) ;
#22734 = LINE ( 'NONE', #6771, #19680 ) ;
#22735 = CARTESIAN_POINT ( 'NONE',  ( 2.620986760973688460E-15, 27.53124999877097068, 13.61880215351699874 ) ) ;
#22736 = CARTESIAN_POINT ( 'NONE',  ( -3.756430356250002323, -25.55312499938548143, 11.16877607737301226 ) ) ;
#22738 = ORIENTED_EDGE ( 'NONE', *, *, #6345, .F. ) ;
#22737 = CARTESIAN_POINT ( 'NONE',  ( 11.44867358849329619, -28.91604871112469510, -6.500000000000000000 ) ) ;
#22739 = DIRECTION ( 'NONE',  ( 0.000000000000000000, 1.000000000000000000, 0.000000000000000000 ) ) ;
#22740 = VERTEX_POINT ( 'NONE', #18714 ) ;
#22741 = CARTESIAN_POINT ( 'NONE',  ( -2.672651547586948120E-15, -25.47812499938548569, 13.33755215474602984 ) ) ;
#22742 = ORIENTED_EDGE ( 'NONE', *, *, #18605, .T. ) ;
#22743 = EDGE_CURVE ( 'NONE', #3260, #7134, #13798, .T. ) ;
#22744 = EDGE_LOOP ( 'NONE', ( #13624, #12701 ) ) ;
#22745 = DIRECTION ( 'NONE',  ( 1.000000000000000000, 0.000000000000000000, 0.000000000000000000 ) ) ;
#22746 = CARTESIAN_POINT ( 'NONE',  ( -1.878215178124996498, 27.65312499938548996, 5.746835883940462963 ) ) ;
#22747 = CARTESIAN_POINT ( 'NONE',  ( -2.999999999999996891, -8.999999999999992895, 0.000000000000000000 ) ) ;
#22748 = CARTESIAN_POINT ( 'NONE',  ( 3.756430356250004099, -6.831223922626973533, 2.990624999385484539 ) ) ;
#22749 = SURFACE_STYLE_FILL_AREA ( #10825 ) ;
#22750 = EDGE_CURVE ( 'NONE', #6676, #12847, #21287, .T. ) ;
#22751 = CARTESIAN_POINT ( 'NONE',  ( 0.000000000000000000, 0.000000000000000000, 1.000000000000000000 ) ) ;
#22752 = CARTESIAN_POINT ( 'NONE',  ( 3.756430356250004099, 28.32812499938548356, 6.831223922626973533 ) ) ;
#22753 = DIRECTION ( 'NONE',  ( -0.000000000000000000, -0.000000000000000000, 1.000000000000000000 ) ) ;
#22754 = UNCERTAINTY_MEASURE_WITH_UNIT (LENGTH_MEASURE( 1.000000000000000082E-05 ), #14774, 'distance_accuracy_value', 'NONE');
#22755 = CARTESIAN_POINT ( 'NONE',  ( -3.756430356249997438, 27.65312499938548640, 11.16877607737301048 ) ) ;
#22756 = CARTESIAN_POINT ( 'NONE',  ( 3.137519842735244810E-15, -26.46249999999999858, 4.999999999999991118 ) ) ;
#22757 = CARTESIAN_POINT ( 'NONE',  ( 4.000000000000003553, 25.88124999877096855, 6.690598923241489970 ) ) ;
#22758 = CYLINDRICAL_SURFACE ( 'NONE', #7618, 0.5000000000000004441 ) ;
#22759 = CARTESIAN_POINT ( 'NONE',  ( -3.756430356250004099, -27.54062499938548569, 6.831223922626973533 ) ) ;
#22760 = CARTESIAN_POINT ( 'NONE',  ( -3.756430356249996994, 29.52812499938548640, 8.999999999999992895 ) ) ;
#22761 = CARTESIAN_POINT ( 'NONE',  ( -27.10000000000000497, -0.5999999999999998668, 19.00000000000000000 ) ) ;
#22762 = CARTESIAN_POINT ( 'NONE',  ( -30.54913349766228592, -5.827558883615738594, -6.500000000000000000 ) ) ;
#22763 = CARTESIAN_POINT ( 'NONE',  ( 3.469446951953614189E-15, 25.00000000000000000, 8.999999999999992895 ) ) ;
#22764 = EDGE_LOOP ( 'NONE', ( #20764, #7636, #19350, #14443 ) ) ;
#22765 = DIRECTION ( 'NONE',  ( 1.000000000000000000, 0.000000000000000000, 0.000000000000000000 ) ) ;
#22767 = ORIENTED_EDGE ( 'NONE', *, *, #19790, .F. ) ;
#22766 = LINE ( 'NONE', #24974, #21684 ) ;
#22768 = EDGE_CURVE ( 'NONE', #14948, #24264, #4611, .T. ) ;
#22769 = ORIENTED_EDGE ( 'NONE', *, *, #19234, .F. ) ;
#22770 = EDGE_LOOP ( 'NONE', ( #11794, #2755, #12419, #9114 ) ) ;
#22771 = ORIENTED_EDGE ( 'NONE', *, *, #8496, .T. ) ;
#22772 = ADVANCED_FACE ( 'NONE', ( #24479 ), #24601, .F. ) ;
#22773 = VERTEX_POINT ( 'NONE', #8785 ) ;
#22774 = CARTESIAN_POINT ( 'NONE',  ( -4.000000000000003553, -27.70000000000000284, 8.999999999999992895 ) ) ;
#22775 = EDGE_CURVE ( 'NONE', #23711, #476, #12579, .T. ) ;
#22776 = ORIENTED_EDGE ( 'NONE', *, *, #1724, .F. ) ;
#22777 = CARTESIAN_POINT ( 'NONE',  ( 26.52310962334750855, 16.23990935651707801, -6.500000000000000000 ) ) ;
#22778 = CARTESIAN_POINT ( 'NONE',  ( 1.878215178125000939, 29.22812499938548569, 12.25316411605952283 ) ) ;
#22779 = CARTESIAN_POINT ( 'NONE',  ( 1.878215178125000939, -12.25316411605952283, 0.5156249993854833402 ) ) ;
#22780 = CARTESIAN_POINT ( 'NONE',  ( -28.41604871112448549, 11.44867358849382910, 1.000000000000000000 ) ) ;
#22781 = CARTESIAN_POINT ( 'NONE',  ( 23.27056975780394765, 17.95817500188513094, 11.16877607737301226 ) ) ;
#22782 = CARTESIAN_POINT ( 'NONE',  ( -1.878215178124998497, 26.45312499938548711, 12.25316411605951927 ) ) ;
#22783 = CARTESIAN_POINT ( 'NONE',  ( -24.67207871933483432, -8.377607117416806304, 20.00001200000000168 ) ) ;
#22784 = VECTOR ( 'NONE', #12392, 1000.000000000000000 ) ;
#22785 = CARTESIAN_POINT ( 'NONE',  ( 2.672651547586948120E-15, -13.33755215474602984, 4.528124999385480187 ) ) ;
#22786 = CARTESIAN_POINT ( 'NONE',  ( 3.469446951953614189E-15, -8.999999999999992895, 18.00000000000000000 ) ) ;
#22787 = CARTESIAN_POINT ( 'NONE',  ( 2.620986760973688460E-15, -13.61880215351699874, 4.387499999999998401 ) ) ;
#22788 = LINE ( 'NONE', #2514, #10089 ) ;
#22789 = LINE ( 'NONE', #18990, #25517 ) ;
#22790 = CARTESIAN_POINT ( 'NONE',  ( 3.735045420075836212E-15, -4.662447845253954171, 2.615624999385482319 ) ) ;
#22791 = CARTESIAN_POINT ( 'NONE',  ( 3.999999999999996447, -26.57500000000000284, 8.999999999999992895 ) ) ;
#22792 = DIRECTION ( 'NONE',  ( 0.000000000000000000, 0.000000000000000000, 1.000000000000000000 ) ) ;
#22793 = VERTEX_POINT ( 'NONE', #1069 ) ;
#22794 = ORIENTED_EDGE ( 'NONE', *, *, #19243, .T. ) ;
#22795 = CARTESIAN_POINT ( 'NONE',  ( 1.878215178125008489, 27.57812499938549422, 5.746835883940462963 ) ) ;
#22796 = ORIENTED_EDGE ( 'NONE', *, *, #1133, .F. ) ;
#22797 = CARTESIAN_POINT ( 'NONE',  ( 26.49999999999999645, 0.5000000000000000000, 19.50000000000000000 ) ) ;
#22798 = EDGE_LOOP ( 'NONE', ( #515, #24167, #18644, #3681 ) ) ;
#22799 = CARTESIAN_POINT ( 'NONE',  ( -1.878215178125004048, -25.77812499938548640, 5.746835883940462963 ) ) ;
#22800 = EDGE_CURVE ( 'NONE', #18677, #855, #13732, .T. ) ;
#22801 = ORIENTED_EDGE ( 'NONE', *, *, #25420, .F. ) ;
#22802 = CARTESIAN_POINT ( 'NONE',  ( 20.92219106202050583, 23.01025686871638598, -2.750000000000000000 ) ) ;
#22803 = EDGE_CURVE ( 'NONE', #15051, #383, #16736, .T. ) ;
#22804 = ORIENTED_EDGE ( 'NONE', *, *, #25823, .F. ) ;
#22805 = LINE ( 'NONE', #9194, #9738 ) ;
#22806 = CARTESIAN_POINT ( 'NONE',  ( -1.878215178124995832, 28.89062499938548356, 5.746835883940462963 ) ) ;
#22807 = EDGE_CURVE ( 'NONE', #14523, #4678, #5747, .T. ) ;
#22808 = CARTESIAN_POINT ( 'NONE',  ( -3.999999999999996447, 28.31874999877096855, 8.999999999999992895 ) ) ;
#22809 = CARTESIAN_POINT ( 'NONE',  ( 3.469446951953614189E-15, 34.00000000000000000, 8.999999999999992895 ) ) ;
#22810 = B_SPLINE_CURVE_WITH_KNOTS ( 'NONE', 3,
 ( #5817, #25702, #25826, #12088, #16035, #11956 ),
 .UNSPECIFIED., .F., .F.,
 ( 4, 2, 4 ),
 ( 2.789812639092967010E-07, 0.0002989033495849343454, 0.0005975277179059593300 ),
 .UNSPECIFIED. ) ;
#22811 = CARTESIAN_POINT ( 'NONE',  ( -1.071796769724487230, 28.22634618820330132, 4.999999999999992006 ) ) ;
#22812 = CARTESIAN_POINT ( 'NONE',  ( 18.01348148472910893, 20.66967886268841426, 12.25316411605951927 ) ) ;
#22813 = CARTESIAN_POINT ( 'NONE',  ( -27.00874656207289348, 15.41874213889432887, 1.000000000000000000 ) ) ;
#22814 = CARTESIAN_POINT ( 'NONE',  ( -3.756430356249997882, 27.20312499938548001, 11.16877607737301226 ) ) ;
#22815 = CARTESIAN_POINT ( 'NONE',  ( -3.999999999999997335, 26.16250000000000142, 11.30940107675849404 ) ) ;
#22816 = CARTESIAN_POINT ( 'NONE',  ( 20.79777820164935775, 15.14092395215691234, 11.30940107675849760 ) ) ;
#22817 = VERTEX_POINT ( 'NONE', #11247 ) ;
#22818 = DIRECTION ( 'NONE',  ( 0.000000000000000000, 0.000000000000000000, 1.000000000000000000 ) ) ;
#22819 = DIRECTION ( 'NONE',  ( 1.000000000000000000, 0.000000000000000000, 0.000000000000000000 ) ) ;
#22820 = CARTESIAN_POINT ( 'NONE',  ( -2.672651547586948120E-15, -26.82812499938548356, 13.33755215474603162 ) ) ;
#22821 = DIRECTION ( 'NONE',  ( 0.000000000000000000, 0.000000000000000000, 1.000000000000000000 ) ) ;
#22822 = CARTESIAN_POINT ( 'NONE',  ( 3.752267015613588906E-15, 29.55624999877096926, 4.381197846482986158 ) ) ;
#22823 = DIRECTION ( 'NONE',  ( 0.000000000000000000, 0.000000000000000000, 1.000000000000000000 ) ) ;
#22825 = EDGE_LOOP ( 'NONE', ( #14380, #14728, #10596, #11972 ) ) ;
#22824 = CARTESIAN_POINT ( 'NONE',  ( 1.878215178125004048, -5.746835883940462963, 0.2156249993854816860 ) ) ;
#22826 = ADVANCED_FACE ( 'NONE', ( #15315 ), #7214, .T. ) ;
#22827 = ORIENTED_EDGE ( 'NONE', *, *, #25723, .F. ) ;
#22828 = CARTESIAN_POINT ( 'NONE',  ( -1.071796769724487230, 28.67634618820330417, 4.999999999999992006 ) ) ;
#22829 =( BOUNDED_CURVE ( )  B_SPLINE_CURVE ( 2, ( #23420, #21467, #19231, #1460, #17676, #5635, #3661, #21714, #25376 ),
 .UNSPECIFIED., .F., .F. ) 
 B_SPLINE_CURVE_WITH_KNOTS ( ( 3, 2, 2, 2, 3 ),
 ( 0.07500000000000001110, 0.08333333333333332871, 0.1000000000000000056, 0.1166666666666666685, 0.1250000000000000000 ),
 .UNSPECIFIED. ) 
 CURVE ( )  GEOMETRIC_REPRESENTATION_ITEM ( )  RATIONAL_B_SPLINE_CURVE ( ( 0.9330127018922192983, 0.9330127018922194093, 1.000000000000000000, 0.8660254037844387076, 1.000000000000000000, 0.8660254037844387076, 1.000000000000000000, 0.9330127018922194093, 0.9330127018922194093 ) ) 
 REPRESENTATION_ITEM ( '' )  );
#22830 = EDGE_CURVE ( 'NONE', #8878, #4940, #21330, .T. ) ;
#22831 = DIRECTION ( 'NONE',  ( -0.000000000000000000, 0.000000000000000000, 1.000000000000000000 ) ) ;
#22832 = ORIENTED_EDGE ( 'NONE', *, *, #15885, .T. ) ;
#22833 = CARTESIAN_POINT ( 'NONE',  ( -1.878215178125000939, -29.67812499938548498, 12.25316411605952283 ) ) ;
#22834 = DIRECTION ( 'NONE',  ( 0.9685831611286301879, -0.2486898871648584586, 0.000000000000000000 ) ) ;
#22835 = DIRECTION ( 'NONE',  ( -0.000000000000000000, -1.000000000000000000, -0.000000000000000000 ) ) ;
#22836 = DIRECTION ( 'NONE',  ( -0.7705132427757840352, 0.6374239897486960738, 0.000000000000000000 ) ) ;
#22837 = CARTESIAN_POINT ( 'NONE',  ( 2.000000000000000000, 25.82500000000000639, 12.46410161513774817 ) ) ;
#22838 = ADVANCED_FACE ( 'NONE', ( #11773 ), #3794, .T. ) ;
#22839 = FACE_OUTER_BOUND ( 'NONE', #13369, .T. ) ;
#22840 = LINE ( 'NONE', #9093, #11268 ) ;
#22841 = DIRECTION ( 'NONE',  ( 0.000000000000000000, 0.000000000000000000, 1.000000000000000000 ) ) ;
#22842 = CARTESIAN_POINT ( 'NONE',  ( 1.999999999999998224, -28.44999999999999929, 12.46410161513774639 ) ) ;
#22843 = CYLINDRICAL_SURFACE ( 'NONE', #21770, 0.5000000000000004441 ) ;
#22844 = CARTESIAN_POINT ( 'NONE',  ( -3.756430356249996994, 25.36562499938548498, 8.999999999999992895 ) ) ;
#22845 = CARTESIAN_POINT ( 'NONE',  ( 1.071796769724487230, -28.22634618820330132, 4.999999999999992006 ) ) ;
#22846 = CARTESIAN_POINT ( 'NONE',  ( 19.20672417798141041, 21.86292155594071218, 12.25316411605951927 ) ) ;
#22847 = CARTESIAN_POINT ( 'NONE',  ( 17.69528343319515784, 20.35148081115446317, 12.25316411605951927 ) ) ;
#22848 = DIRECTION ( 'NONE',  ( 0.000000000000000000, 1.000000000000000000, 0.000000000000000000 ) ) ;
#22849 = DIRECTION ( 'NONE',  ( 0.000000000000000000, -0.000000000000000000, 1.000000000000000000 ) ) ;
#22850 = CARTESIAN_POINT ( 'NONE',  ( 3.756430356250004099, 28.77812499938548285, 6.831223922626973533 ) ) ;
#22851 = CARTESIAN_POINT ( 'NONE',  ( 0.4999838450259764255, -31.09598070739550124, 1.000000000000000000 ) ) ;
#22852 = CARTESIAN_POINT ( 'NONE',  ( -1.999999999999994893, 25.54374999877097352, 5.535898384862237620 ) ) ;
#22853 = DIRECTION ( 'NONE',  ( 0.000000000000000000, 0.000000000000000000, 1.000000000000000000 ) ) ;
#22854 = ORIENTED_EDGE ( 'NONE', *, *, #1964, .T. ) ;
#22855 = DIRECTION ( 'NONE',  ( -0.000000000000000000, -0.000000000000000000, -1.000000000000000000 ) ) ;
#22856 = CARTESIAN_POINT ( 'NONE',  ( 2.620986760973688460E-15, 28.88124999877096855, 13.61880215351699874 ) ) ;
#22857 = CARTESIAN_POINT ( 'NONE',  ( -3.756430356250004099, -28.32812499938548356, 6.831223922626973533 ) ) ;
#22859 = ORIENTED_EDGE ( 'NONE', *, *, #3740, .T. ) ;
#22858 = DIRECTION ( 'NONE',  ( 0.8090169943749474513, -0.5877852522924730261, 0.000000000000000000 ) ) ;
#22860 = CARTESIAN_POINT ( 'NONE',  ( -3.834746474454188013E-15, -25.95624999877096428, 4.999999999999992006 ) ) ;
#22861 = ORIENTED_EDGE ( 'NONE', *, *, #20313, .T. ) ;
#22862 = CARTESIAN_POINT ( 'NONE',  ( 1.878215178124998497, -29.04062499938548569, 12.25316411605951927 ) ) ;
#22863 = ORIENTED_EDGE ( 'NONE', *, *, #6317, .T. ) ;
#22864 = VERTEX_POINT ( 'NONE', #11388 ) ;
#22865 = CARTESIAN_POINT ( 'NONE',  ( 8.012344526598182026E-15, 28.51562499938549067, 4.662447845253954171 ) ) ;
#22866 = EDGE_CURVE ( 'NONE', #17279, #7474, #1687, .T. ) ;
#22867 = CARTESIAN_POINT ( 'NONE',  ( -25.99519186311192342, 0.5000000000000000000, 20.00000000000000000 ) ) ;
#22868 = CARTESIAN_POINT ( 'NONE',  ( 3.756430356250002323, -11.16877607737301226, 1.565624999385482941 ) ) ;
#22869 = EDGE_CURVE ( 'NONE', #4035, #15232, #2731, .T. ) ;
#22870 = DIRECTION ( 'NONE',  ( 0.1873813145857330109, 0.9822872507286871668, 0.000000000000000000 ) ) ;
#22871 = CARTESIAN_POINT ( 'NONE',  ( -3.756430356249997882, 28.10312499938548569, 11.16877607737301226 ) ) ;
#22872 = CARTESIAN_POINT ( 'NONE',  ( -3.999999999999996447, -8.999999999999992895, 1.968749998770967569 ) ) ;
#22873 = DIRECTION ( 'NONE',  ( 0.000000000000000000, 0.000000000000000000, 1.000000000000000000 ) ) ;
#22874 = CARTESIAN_POINT ( 'NONE',  ( -1.878215178124998497, 28.59062499938548285, 12.25316411605951927 ) ) ;
#22875 = FILL_AREA_STYLE ('',( #20524 ) ) ;
#22876 = DIRECTION ( 'NONE',  ( 0.000000000000000000, 0.000000000000000000, -1.000000000000000000 ) ) ;
#22877 = CARTESIAN_POINT ( 'NONE',  ( 3.878215178125003604, -8.999999999999992895, 0.07031249969274150358 ) ) ;
#22878 = DIRECTION ( 'NONE',  ( -0.7071067811865487940, -0.7071067811865463515, 0.000000000000000000 ) ) ;
#22879 = CARTESIAN_POINT ( 'NONE',  ( 3.756430356249995661, -27.69062499938548427, 6.831223922626973533 ) ) ;
#22880 = CARTESIAN_POINT ( 'NONE',  ( -1.878215178124995832, 25.40312499938548640, 5.746835883940462963 ) ) ;
#22881 = FACE_OUTER_BOUND ( 'NONE', #24724, .T. ) ;
#22882 = DIRECTION ( 'NONE',  ( 1.000000000000000000, 0.000000000000000000, 0.000000000000000000 ) ) ;
#22883 = LINE ( 'NONE', #15296, #13911 ) ;
#22884 = ORIENTED_EDGE ( 'NONE', *, *, #17433, .T. ) ;
#22885 = CARTESIAN_POINT ( 'NONE',  ( -27.10000000000000497, -0.5999999999999998668, 19.00000000000000000 ) ) ;
#22887 = ORIENTED_EDGE ( 'NONE', *, *, #7037, .T. ) ;
#22886 = CARTESIAN_POINT ( 'NONE',  ( -3.999999999999996447, -8.999999999999992895, 2.925000000000000711 ) ) ;
#22888 = ORIENTED_EDGE ( 'NONE', *, *, #3482, .F. ) ;
#22889 = CIRCLE ( 'NONE', #7445, 0.4999999999999997224 ) ;
#22890 = ORIENTED_EDGE ( 'NONE', *, *, #6520, .F. ) ;
#22891 = ORIENTED_EDGE ( 'NONE', *, *, #15019, .F. ) ;
#22892 = ORIENTED_EDGE ( 'NONE', *, *, #7271, .T. ) ;
#22893 = LINE ( 'NONE', #20940, #10529 ) ;
#22895 = ORIENTED_EDGE ( 'NONE', *, *, #12571, .F. ) ;
#22894 = AXIS2_PLACEMENT_3D ( 'NONE', #24787, #13018, #18905 ) ;
#22896 = DIRECTION ( 'NONE',  ( 0.000000000000000000, 0.000000000000000000, -1.000000000000000000 ) ) ;
#22897 = CYLINDRICAL_SURFACE ( 'NONE', #24777, 31.10000000000000142 ) ;
#22898 = EDGE_CURVE ( 'NONE', #18701, #2418, #1576, .T. ) ;
#22899 = CARTESIAN_POINT ( 'NONE',  ( -1.878215178124995832, -5.746835883940462963, 0.7406249993854828739 ) ) ;
#22900 = FACE_OUTER_BOUND ( 'NONE', #8975, .T. ) ;
#22901 = CARTESIAN_POINT ( 'NONE',  ( 17.48087792458429135, 22.79327268050296240, 6.831223922626973533 ) ) ;
#22902 = EDGE_CURVE ( 'NONE', #25109, #11111, #22159, .T. ) ;
#22903 = CARTESIAN_POINT ( 'NONE',  ( -3.756430356249997882, 26.41562499938548569, 11.16877607737301226 ) ) ;
#22904 = CARTESIAN_POINT ( 'NONE',  ( 13.02991752792604174, -22.56362157461193263, 20.00001200000000168 ) ) ;
#22905 = CIRCLE ( 'NONE', #17061, 0.5000000000000002220 ) ;
#22906 = CARTESIAN_POINT ( 'NONE',  ( -3.999999999999996447, -8.999999999999992895, 0.2249999999999995060 ) ) ;
#22907 = FACE_OUTER_BOUND ( 'NONE', #9026, .T. ) ;
#22909 = EDGE_CURVE ( 'NONE', #24428, #9293, #11437, .T. ) ;
#22908 = CARTESIAN_POINT ( 'NONE',  ( -3.999999999999996447, -8.999999999999992895, 4.275000000000001243 ) ) ;
#22910 = CYLINDRICAL_SURFACE ( 'NONE', #15951, 31.10000000000000142 ) ;
#22911 = CARTESIAN_POINT ( 'NONE',  ( -4.000000000000003553, -25.39374999877096784, 8.999999999999992895 ) ) ;
#22912 = CARTESIAN_POINT ( 'NONE',  ( 1.878215178125004048, -5.746835883940462963, 3.928124999385485872 ) ) ;
#22913 = AXIS2_PLACEMENT_3D ( 'NONE', #15081, #20701, #17308 ) ;
#22914 = DIRECTION ( 'NONE',  ( 1.000000000000000000, 0.000000000000000000, 0.000000000000000000 ) ) ;
#22915 = CIRCLE ( 'NONE', #25422, 31.10000000000000142 ) ;
#22916 = CARTESIAN_POINT ( 'NONE',  ( -10.94867358849371541, -28.91604871112453168, -6.500000000000000000 ) ) ;
#22917 = ORIENTED_EDGE ( 'NONE', *, *, #5735, .F. ) ;
#22918 = ORIENTED_EDGE ( 'NONE', *, *, #8020, .F. ) ;
#22919 = ORIENTED_EDGE ( 'NONE', *, *, #10822, .T. ) ;
#22920 = CARTESIAN_POINT ( 'NONE',  ( 0.000000000000000000, 0.000000000000000000, 19.00000000000000000 ) ) ;
#22921 = EDGE_LOOP ( 'NONE', ( #3971, #22457, #5456, #20119 ) ) ;
#22922 = CARTESIAN_POINT ( 'NONE',  ( -17.08421000182784866, -25.98730014090430984, 1.000000000000000000 ) ) ;
#22923 = EDGE_LOOP ( 'NONE', ( #18254, #15633, #193, #22742 ) ) ;
#22924 = CARTESIAN_POINT ( 'NONE',  ( -16.66421332384646448, 26.25859848311288403, -6.500000000000000000 ) ) ;
#22925 = AXIS2_PLACEMENT_3D ( 'NONE', #1263, #20628, #14752 ) ;
#22926 = ORIENTED_EDGE ( 'NONE', *, *, #8450, .T. ) ;
#22927 = CARTESIAN_POINT ( 'NONE',  ( 3.756430356250004987, 25.25312499938548427, 8.999999999999992895 ) ) ;
#22928 = CARTESIAN_POINT ( 'NONE',  ( 3.756430356250002323, 29.60312499938548569, 11.16877607737301226 ) ) ;
#22929 = CARTESIAN_POINT ( 'NONE',  ( -29.72853858738272592, 9.133673601486785643, 1.000000000000000000 ) ) ;
#22930 = VECTOR ( 'NONE', #16683, 1000.000000000000000 ) ;
#22931 = AXIS2_PLACEMENT_3D ( 'NONE', #7789, #13560, #13675 ) ;
#22932 = CYLINDRICAL_SURFACE ( 'NONE', #8415, 0.5000000000000004441 ) ;
#22933 = LINE ( 'NONE', #6715, #14175 ) ;
#22934 = CARTESIAN_POINT ( 'NONE',  ( 17.27101936448323016, 19.92721674244253549, 5.746835883940462963 ) ) ;
#22935 = DIRECTION ( 'NONE',  ( 1.000000000000000000, 0.000000000000000000, 0.000000000000000000 ) ) ;
#22936 = EDGE_CURVE ( 'NONE', #9588, #13852, #2933, .T. ) ;
#22937 = CARTESIAN_POINT ( 'NONE',  ( -1.999999999999998224, 26.20000000000000284, 12.46410161513774639 ) ) ;
#22938 = EDGE_CURVE ( 'NONE', #18492, #6156, #21326, .T. ) ;
#22939 = CARTESIAN_POINT ( 'NONE',  ( 18.54381157061901675, 21.20000894857831852, 5.746835883940462963 ) ) ;
#22940 = CARTESIAN_POINT ( 'NONE',  ( 4.000000000000003553, 26.74374999877096926, 8.999999999999992895 ) ) ;
#22941 = AXIS2_PLACEMENT_3D ( 'NONE', #10457, #20268, #12556 ) ;
#22942 = VERTEX_POINT ( 'NONE', #9689 ) ;
#22943 = CARTESIAN_POINT ( 'NONE',  ( -3.999999999999994671, 26.93124999877097281, 6.690598923241487306 ) ) ;
#22944 = EDGE_CURVE ( 'NONE', #23846, #18705, #25641, .T. ) ;
#22946 = CARTESIAN_POINT ( 'NONE',  ( 1.878215178124995832, -28.44062499938548427, 5.746835883940462963 ) ) ;
#22945 = CIRCLE ( 'NONE', #11662, 0.4999999999999998335 ) ;
#22947 = DIRECTION ( 'NONE',  ( 1.000000000000000000, 0.000000000000000000, 0.000000000000000000 ) ) ;
#22948 = AXIS2_PLACEMENT_3D ( 'NONE', #25557, #23847, #1496 ) ;
#22949 = CARTESIAN_POINT ( 'NONE',  ( -3.999999999999996003, 29.63124999877096499, 6.690598923241487306 ) ) ;
#22950 = CARTESIAN_POINT ( 'NONE',  ( -27.10000000000000497, -0.5999999999999998668, 19.00000000000000000 ) ) ;
#22952 = EDGE_LOOP ( 'NONE', ( #13373, #4379, #5075, #21867 ) ) ;
#22951 = CARTESIAN_POINT ( 'NONE',  ( 6.009258394948636914E-15, 29.41562499938548925, 4.662447845253954171 ) ) ;
#22953 = VERTEX_POINT ( 'NONE', #3272 ) ;
#22954 = DIRECTION ( 'NONE',  ( 1.000000000000000000, 0.000000000000000000, 0.000000000000000000 ) ) ;
#22955 = CARTESIAN_POINT ( 'NONE',  ( 1.500000000000000222, 0.000000000000000000, 17.69999999999999929 ) ) ;
#22956 = ORIENTED_EDGE ( 'NONE', *, *, #9041, .F. ) ;
#22957 = CARTESIAN_POINT ( 'NONE',  ( -3.756430356250002323, -28.81562499938548427, 11.16877607737301403 ) ) ;
#22958 = DIRECTION ( 'NONE',  ( 0.4257792915650852050, 0.9048270524660135816, 0.000000000000000000 ) ) ;
#22959 = CARTESIAN_POINT ( 'NONE',  ( 0.000000000000000000, 0.000000000000000000, -6.500000000000000000 ) ) ;
#22960 = PRESENTATION_LAYER_ASSIGNMENT (  '', '', ( #5405 ) ) ;
#22961 = CARTESIAN_POINT ( 'NONE',  ( 3.469446951953614189E-15, 39.50000000000000000, 8.999999999999992895 ) ) ;
#22962 = CARTESIAN_POINT ( 'NONE',  ( 2.003086131649545506E-15, 29.07812499938549067, 13.33755215474602984 ) ) ;
#22963 =( GEOMETRIC_REPRESENTATION_CONTEXT ( 3 ) GLOBAL_UNCERTAINTY_ASSIGNED_CONTEXT ( ( #1040 ) ) GLOBAL_UNIT_ASSIGNED_CONTEXT ( ( #9039, #24987, #7072 ) ) REPRESENTATION_CONTEXT ( 'NONE', 'WORKASPACE' ) );
#22964 = CIRCLE ( 'NONE', #25054, 31.10000000000000142 ) ;
#22965 = ADVANCED_FACE ( 'NONE', ( #1330 ), #17291, .F. ) ;
#22966 = CARTESIAN_POINT ( 'NONE',  ( 4.000000000000002665, 29.03124999877096712, 6.690598923241489970 ) ) ;
#22967 = PRESENTATION_STYLE_ASSIGNMENT (( #6882 ) ) ;
#22968 =( BOUNDED_CURVE ( )  B_SPLINE_CURVE ( 2, ( #1821, #9279, #19460, #23390, #23143 ),
 .UNSPECIFIED., .F., .F. ) 
 B_SPLINE_CURVE_WITH_KNOTS ( ( 3, 2, 3 ),
 ( 0.9749999999999999778, 0.9833333333333332815, 0.9889400238386636399 ),
 .UNSPECIFIED. ) 
 CURVE ( )  GEOMETRIC_REPRESENTATION_ITEM ( )  RATIONAL_B_SPLINE_CURVE ( ( 0.9330127018922194093, 0.9330127018922194093, 1.000000000000000000, 0.9549307542065648136, 0.9401842259098239785 ) ) 
 REPRESENTATION_ITEM ( '' )  );
#22969 = DIRECTION ( 'NONE',  ( 0.000000000000000000, 0.000000000000000000, 1.000000000000000000 ) ) ;
#22970 = EDGE_CURVE ( 'NONE', #2251, #7412, #6139, .T. ) ;
#22971 = DIRECTION ( 'NONE',  ( 0.000000000000000000, 1.000000000000000000, 0.000000000000000000 ) ) ;
#22972 = CARTESIAN_POINT ( 'NONE',  ( -1.878215178124998497, 25.89062499938548356, 12.25316411605951927 ) ) ;
#22973 = VECTOR ( 'NONE', #14725, 1000.000000000000000 ) ;
#22974 = CARTESIAN_POINT ( 'NONE',  ( 2.000000000000003997, 25.52500000000000213, 5.535898384862238508 ) ) ;
#22975 = CARTESIAN_POINT ( 'NONE',  ( 19.46311415215975771, 16.63468702741349858, 5.535898384862238508 ) ) ;
#22976 = CARTESIAN_POINT ( 'NONE',  ( 19.51172774249728192, 22.34015486724339183, 5.535898384862237620 ) ) ;
#22977 = LINE ( 'NONE', #24677, #2964 ) ;
#22978 =( BOUNDED_SURFACE ( )  B_SPLINE_SURFACE ( 1, 2, ( 
 ( #14852, #988, #22824, #19023, #9081, #24647, #17065, #10648, #14726, #12877, #20854, #10220, #176, #12443, #18217, #10337, #22127, #20029, #8653, #20410, #689, #16126, #298, #2384, #18098, #24088, #10097, #24220, #8269, #16634, #22384, #18338, #18602, #14540, #6307, #14679, #14159, #6438, #434, #8147, #4077, #4214, #6171, #16392, #2134, #16251, #10480, #24360, #12050, #10611, #2512, #18479, #20289, #12580, #14423, #12193, #14301, #22266, #6686, #4345, #2264, #568, #20163, #12321, #24603, #4598, #8404, #8538, #4466, #16519, #24480, #6559, #22520, #20560, #2649, #12718, #1332, #13109, #19230, #8787, #18863, #20954, #10730, #16776, #2769, #16909, #951, #9308, #15069, #11006, #11249, #7216, #24874, #7339, #6829, #24992, #3037, #18716, #22660, #14811, #808, #9044, #17293, #7079, #20686, #19103, #12837, #17026, #23044, #6953, #25259, #5130, #4992, #18985, #4748, #24744, #12970, #22785, #21080, #1188, #9169 ),
 ( #8929, #3275, #17159, #25131, #14932, #4861, #22906, #13227, #10862, #1070, #20812, #2895, #3156, #11125, #15199, #23168, #5248, #21198, #11514, #3411, #21713, #13496, #15827, #15317, #23285, #7459, #13735, #21580, #9813, #11390, #23801, #3660, #15449, #15708, #19365, #25643, #1967, #1717, #19483, #23672, #9430, #9691, #5369, #17675, #13360, #5889, #5634, #21332, #1578, #21848, #19754, #17796, #9549, #9931, #17538, #13873, #3541, #25511, #1459, #23419, #3797, #7724, #5749, #1851, #21466, #17917, #7599, #17412, #11776, #15584, #3930, #25375, #5506, #23553, #25762, #11637, #7843, #13614, #11899, #19613, #19867, #9, #14681, #8539, #14813, #3039, #2651, #6688, #24877, #16636, #6955, #18339, #18604, #2771, #16393, #4600, #24746, #12720, #435, #14935, #811, #6831, #8655, #953, #4750, #4468, #6561, #14542, #20957, #22522, #16521, #16778, #12444, #24481, #22908, #18865, #20411, #22787, #8405, #12582, #14424 ) ),
 .UNSPECIFIED., .F., .F., .F. ) 
 B_SPLINE_SURFACE_WITH_KNOTS ( ( 2, 2 ),
 ( 3, 2, 2, 2, 2, 2, 2, 2, 2, 2, 2, 2, 2, 2, 2, 2, 2, 2, 2, 2, 2, 2, 2, 2, 2, 2, 2, 2, 2, 2, 2, 2, 2, 2, 2, 2, 2, 2, 2, 2, 2, 2, 2, 2, 2, 2, 2, 2, 2, 2, 2, 2, 2, 2, 2, 2, 2, 2, 2, 2, 3 ),
 ( 0.000000000000000000, 1.000000000000000000 ),
 ( 0.000000000000000000, 0.01666666666666666644, 0.03333333333333333287, 0.05000000000000000278, 0.06666666666666666574, 0.08333333333333332871, 0.1000000000000000056, 0.1166666666666666685, 0.1333333333333333315, 0.1499999999999999944, 0.1666666666666666574, 0.1833333333333333204, 0.2000000000000000111, 0.2166666666666666741, 0.2333333333333333370, 0.2500000000000000000, 0.2666666666666666630, 0.2833333333333333259, 0.2999999999999999889, 0.3166666666666666519, 0.3333333333333333148, 0.3499999999999999778, 0.3666666666666666408, 0.3833333333333333592, 0.4000000000000000222, 0.4166666666666666852, 0.4333333333333333481, 0.4500000000000000111, 0.4666666666666666741, 0.4833333333333333370, 0.5000000000000000000, 0.5166666666666667185, 0.5333333333333333259, 0.5500000000000000444, 0.5666666666666666519, 0.5833333333333333703, 0.5999999999999999778, 0.6166666666666666963, 0.6333333333333333037, 0.6500000000000000222, 0.6666666666666666297, 0.6833333333333333481, 0.6999999999999999556, 0.7166666666666666741, 0.7333333333333332815, 0.7500000000000000000, 0.7666666666666667185, 0.7833333333333333259, 0.8000000000000000444, 0.8166666666666666519, 0.8333333333333333703, 0.8499999999999999778, 0.8666666666666666963, 0.8833333333333333037, 0.9000000000000000222, 0.9166666666666666297, 0.9333333333333333481, 0.9499999999999999556, 0.9666666666666666741, 0.9833333333333332815, 1.000000000000000000 ),
 .UNSPECIFIED. ) 
 GEOMETRIC_REPRESENTATION_ITEM ( )  RATIONAL_B_SPLINE_SURFACE ( (
 ( 1.000000000000000000, 0.8660254037844387076, 1.000000000000000000, 0.8660254037844387076, 1.000000000000000000, 0.8660254037844387076, 1.000000000000000000, 0.8660254037844387076, 1.000000000000000000, 0.8660254037844387076, 1.000000000000000000, 0.8660254037844387076, 1.000000000000000000, 0.8660254037844387076, 1.000000000000000000, 0.8660254037844387076, 1.000000000000000000, 0.8660254037844387076, 1.000000000000000000, 0.8660254037844387076, 1.000000000000000000, 0.8660254037844387076, 1.000000000000000000, 0.8660254037844387076, 1.000000000000000000, 0.8660254037844387076, 1.000000000000000000, 0.8660254037844387076, 1.000000000000000000, 0.8660254037844387076, 1.000000000000000000, 0.8660254037844387076, 1.000000000000000000, 0.8660254037844387076, 1.000000000000000000, 0.8660254037844387076, 1.000000000000000000, 0.8660254037844387076, 1.000000000000000000, 0.8660254037844387076, 1.000000000000000000, 0.8660254037844387076, 1.000000000000000000, 0.8660254037844387076, 1.000000000000000000, 0.8660254037844387076, 1.000000000000000000, 0.8660254037844387076, 1.000000000000000000, 0.8660254037844387076, 1.000000000000000000, 0.8660254037844387076, 1.000000000000000000, 0.8660254037844387076, 1.000000000000000000, 0.8660254037844387076, 1.000000000000000000, 0.8660254037844387076, 1.000000000000000000, 0.8660254037844387076, 1.000000000000000000, 0.8660254037844387076, 1.000000000000000000, 0.8660254037844387076, 1.000000000000000000, 0.8660254037844387076, 1.000000000000000000, 0.8660254037844387076, 1.000000000000000000, 0.8660254037844387076, 1.000000000000000000, 0.8660254037844387076, 1.000000000000000000, 0.8660254037844387076, 1.000000000000000000, 0.8660254037844387076, 1.000000000000000000, 0.8660254037844387076, 1.000000000000000000, 0.8660254037844387076, 1.000000000000000000, 0.8660254037844387076, 1.000000000000000000, 0.8660254037844387076, 1.000000000000000000, 0.8660254037844387076, 1.000000000000000000, 0.8660254037844387076, 1.000000000000000000, 0.8660254037844387076, 1.000000000000000000, 0.8660254037844387076, 1.000000000000000000, 0.8660254037844387076, 1.000000000000000000, 0.8660254037844387076, 1.000000000000000000, 0.8660254037844387076, 1.000000000000000000, 0.8660254037844387076, 1.000000000000000000, 0.8660254037844387076, 1.000000000000000000, 0.8660254037844387076, 1.000000000000000000, 0.8660254037844387076, 1.000000000000000000, 0.8660254037844387076, 1.000000000000000000, 0.8660254037844387076, 1.000000000000000000, 0.8660254037844387076, 1.000000000000000000, 0.8660254037844387076, 1.000000000000000000, 0.8660254037844387076, 1.000000000000000000, 0.8660254037844387076, 1.000000000000000000, 0.8660254037844387076, 1.000000000000000000),
 ( 1.000000000000000000, 0.8660254037844387076, 1.000000000000000000, 0.8660254037844387076, 1.000000000000000000, 0.8660254037844387076, 1.000000000000000000, 0.8660254037844387076, 1.000000000000000000, 0.8660254037844387076, 1.000000000000000000, 0.8660254037844387076, 1.000000000000000000, 0.8660254037844387076, 1.000000000000000000, 0.8660254037844387076, 1.000000000000000000, 0.8660254037844387076, 1.000000000000000000, 0.8660254037844387076, 1.000000000000000000, 0.8660254037844387076, 1.000000000000000000, 0.8660254037844387076, 1.000000000000000000, 0.8660254037844387076, 1.000000000000000000, 0.8660254037844387076, 1.000000000000000000, 0.8660254037844387076, 1.000000000000000000, 0.8660254037844387076, 1.000000000000000000, 0.8660254037844387076, 1.000000000000000000, 0.8660254037844387076, 1.000000000000000000, 0.8660254037844387076, 1.000000000000000000, 0.8660254037844387076, 1.000000000000000000, 0.8660254037844387076, 1.000000000000000000, 0.8660254037844387076, 1.000000000000000000, 0.8660254037844387076, 1.000000000000000000, 0.8660254037844387076, 1.000000000000000000, 0.8660254037844387076, 1.000000000000000000, 0.8660254037844387076, 1.000000000000000000, 0.8660254037844387076, 1.000000000000000000, 0.8660254037844387076, 1.000000000000000000, 0.8660254037844387076, 1.000000000000000000, 0.8660254037844387076, 1.000000000000000000, 0.8660254037844387076, 1.000000000000000000, 0.8660254037844387076, 1.000000000000000000, 0.8660254037844387076, 1.000000000000000000, 0.8660254037844387076, 1.000000000000000000, 0.8660254037844387076, 1.000000000000000000, 0.8660254037844387076, 1.000000000000000000, 0.8660254037844387076, 1.000000000000000000, 0.8660254037844387076, 1.000000000000000000, 0.8660254037844387076, 1.000000000000000000, 0.8660254037844387076, 1.000000000000000000, 0.8660254037844387076, 1.000000000000000000, 0.8660254037844387076, 1.000000000000000000, 0.8660254037844387076, 1.000000000000000000, 0.8660254037844387076, 1.000000000000000000, 0.8660254037844387076, 1.000000000000000000, 0.8660254037844387076, 1.000000000000000000, 0.8660254037844387076, 1.000000000000000000, 0.8660254037844387076, 1.000000000000000000, 0.8660254037844387076, 1.000000000000000000, 0.8660254037844387076, 1.000000000000000000, 0.8660254037844387076, 1.000000000000000000, 0.8660254037844387076, 1.000000000000000000, 0.8660254037844387076, 1.000000000000000000, 0.8660254037844387076, 1.000000000000000000, 0.8660254037844387076, 1.000000000000000000, 0.8660254037844387076, 1.000000000000000000, 0.8660254037844387076, 1.000000000000000000, 0.8660254037844387076, 1.000000000000000000, 0.8660254037844387076, 1.000000000000000000, 0.8660254037844387076, 1.000000000000000000) ) ) 
 REPRESENTATION_ITEM ( '' )  SURFACE ( )  );
#22979 = CARTESIAN_POINT ( 'NONE',  ( -3.756430356249996994, 28.96562499938548285, 8.999999999999992895 ) ) ;
#22980 = AXIS2_PLACEMENT_3D ( 'NONE', #17027, #2770, #10731 ) ;
#22981 = CARTESIAN_POINT ( 'NONE',  ( 23.96296185032695192, -19.82388608118436935, 1.000000000000000000 ) ) ;
#22982 = CIRCLE ( 'NONE', #24, 0.5000000000000001110 ) ;
#22983 = CARTESIAN_POINT ( 'NONE',  ( 16.57931677857143882, 21.89171153449011697, 11.16877607737301048 ) ) ;
#22984 = CYLINDRICAL_SURFACE ( 'NONE', #19627, 4.000000000000000000 ) ;
#22985 = ORIENTED_EDGE ( 'NONE', *, *, #5952, .T. ) ;
#22986 = DIRECTION ( 'NONE',  ( -0.7289686274214034478, 0.6845471059286972748, 0.000000000000000000 ) ) ;
#22987 = CARTESIAN_POINT ( 'NONE',  ( -3.999999999999997335, 27.00624999877096499, 11.30940107675849404 ) ) ;
#22988 = CARTESIAN_POINT ( 'NONE',  ( 3.756430356249995661, -28.92812499938548143, 6.831223922626973533 ) ) ;
#22990 = VERTEX_POINT ( 'NONE', #22351 ) ;
#22989 = DIRECTION ( 'NONE',  ( -0.000000000000000000, 0.000000000000000000, 1.000000000000000000 ) ) ;
#22991 = CARTESIAN_POINT ( 'NONE',  ( -3.756430356249997438, 26.86562499938548498, 11.16877607737301048 ) ) ;
#22992 = EDGE_CURVE ( 'NONE', #8478, #10323, #2231, .T. ) ;
#22993 = ORIENTED_EDGE ( 'NONE', *, *, #5525, .F. ) ;
#22994 = CARTESIAN_POINT ( 'NONE',  ( -1.878215178125000939, -28.66562499938548569, 12.25316411605952283 ) ) ;
#22995 = EDGE_LOOP ( 'NONE', ( #2757, #1551, #5473, #5928 ) ) ;
#22996 = VERTEX_POINT ( 'NONE', #3928 ) ;
#22997 = CARTESIAN_POINT ( 'NONE',  ( 18.35858150987925086, 23.72704589961136534, 10.28786097927511101 ) ) ;
#22998 = CARTESIAN_POINT ( 'NONE',  ( 1.878215178125001605, 28.77812499938549351, 12.25316411605952283 ) ) ;
#22999 = VECTOR ( 'NONE', #22182, 1000.000000000000000 ) ;
#23000 = CARTESIAN_POINT ( 'NONE',  ( -3.756430356249996105, -6.831223922626973533, 1.228124999385478144 ) ) ;
#23001 = CIRCLE ( 'NONE', #17167, 31.10000000000000142 ) ;
#23002 = CARTESIAN_POINT ( 'NONE',  ( 1.878215178125000939, -12.25316411605952283, 4.678124999385483207 ) ) ;
#23003 =( NAMED_UNIT ( * ) SI_UNIT ( $, .STERADIAN. ) SOLID_ANGLE_UNIT ( ) );
#23004 = CARTESIAN_POINT ( 'NONE',  ( -29.07785765677936851, -9.610428525060582317, -6.500000000000000000 ) ) ;
#23005 = CARTESIAN_POINT ( 'NONE',  ( 3.756430356250004099, 29.22812499938548925, 6.831223922626973533 ) ) ;
#23006 = VECTOR ( 'NONE', #8237, 1000.000000000000000 ) ;
#23007 = CARTESIAN_POINT ( 'NONE',  ( 21.90263254725334363, 19.07420542250708451, 12.46410161513774817 ) ) ;
#23008 = CARTESIAN_POINT ( 'NONE',  ( -0.7500000000000000000, 0.000000000000000000, 17.69999999999999929 ) ) ;
#23009 = UNCERTAINTY_MEASURE_WITH_UNIT (LENGTH_MEASURE( 1.000000000000000082E-05 ), #22125, 'distance_accuracy_value', 'NONE');
#23010 = PRODUCT_DEFINITION_CONTEXT ( 'detailed design', #13960, 'design' ) ;
#23011 = CARTESIAN_POINT ( 'NONE',  ( 21.21320343559646915, 21.21320343559638744, 8.999999999999992895 ) ) ;
#23012 =( LENGTH_UNIT ( ) NAMED_UNIT ( * ) SI_UNIT ( .MILLI., .METRE. ) );
#23013 = CARTESIAN_POINT ( 'NONE',  ( 0.000000000000000000, 0.000000000000000000, -6.500000000000000000 ) ) ;
#23014 = DIRECTION ( 'NONE',  ( 0.000000000000000000, -0.000000000000000000, 1.000000000000000000 ) ) ;
#23015 = CARTESIAN_POINT ( 'NONE',  ( 17.29197772466794802, 18.80772725251993194, 4.999999999999994671 ) ) ;
#23016 = CARTESIAN_POINT ( 'NONE',  ( 1.878215178124998497, -26.45312499938548711, 12.25316411605951927 ) ) ;
#23017 = CARTESIAN_POINT ( 'NONE',  ( -1.878215178124998497, 26.00312499938548783, 12.25316411605951927 ) ) ;
#23018 = ADVANCED_FACE ( 'NONE', ( #22088 ), #12013, .T. ) ;
#23019 = CARTESIAN_POINT ( 'NONE',  ( 3.469446951953614189E-15, 35.50000000000000711, 8.999999999999992895 ) ) ;
#23020 = VECTOR ( 'NONE', #15992, 1000.000000000000000 ) ;
#23021 = CARTESIAN_POINT ( 'NONE',  ( 5.335677986744567391, -30.63887302793249745, -2.750000000000000000 ) ) ;
#23022 = DIRECTION ( 'NONE',  ( -0.000000000000000000, 1.000000000000000000, -0.000000000000000000 ) ) ;
#23023 = ORIENTED_EDGE ( 'NONE', *, *, #9968, .F. ) ;
#23024 = CARTESIAN_POINT ( 'NONE',  ( -5.312859100616741159, 38.96936022227531282, 7.461857399205459096 ) ) ;
#23026 = ORIENTED_EDGE ( 'NONE', *, *, #4246, .F. ) ;
#23025 = DIRECTION ( 'NONE',  ( 0.000000000000000000, 0.000000000000000000, 1.000000000000000000 ) ) ;
#23027 = CIRCLE ( 'NONE', #13829, 0.4999999999999993339 ) ;
#23028 = VECTOR ( 'NONE', #13580, 1000.000000000000000 ) ;
#23029 = ORIENTED_EDGE ( 'NONE', *, *, #25163, .F. ) ;
#23030 = VERTEX_POINT ( 'NONE', #394 ) ;
#23031 = VERTEX_POINT ( 'NONE', #2352 ) ;
#23032 = ORIENTED_EDGE ( 'NONE', *, *, #18300, .T. ) ;
#23033 = CARTESIAN_POINT ( 'NONE',  ( 0.000000000000000000, 0.000000000000000000, 20.00000000000000000 ) ) ;
#23034 = DIRECTION ( 'NONE',  ( 1.000000000000000000, 0.000000000000000000, 0.000000000000000000 ) ) ;
#23035 = CARTESIAN_POINT ( 'NONE',  ( -1.878215178124995832, 28.10312499938548569, 5.746835883940462963 ) ) ;
#23036 = CIRCLE ( 'NONE', #15104, 0.5000000000000002220 ) ;
#23037 = CARTESIAN_POINT ( 'NONE',  ( -3.756430356249996994, -8.999999999999992895, 1.265624999385484006 ) ) ;
#23038 = CARTESIAN_POINT ( 'NONE',  ( 2.620986760973688460E-15, -13.61880215351699874, 2.531249998770966236 ) ) ;
#23039 = CARTESIAN_POINT ( 'NONE',  ( 21.38562447863985483, 18.72942710068040739, 5.746835883940462963 ) ) ;
#23040 = VECTOR ( 'NONE', #24820, 1000.000000000000000 ) ;
#23041 = CARTESIAN_POINT ( 'NONE',  ( -1.878215178124998497, 25.55312499938548854, 12.25316411605951927 ) ) ;
#23042 = AXIS2_PLACEMENT_3D ( 'NONE', #14869, #6495, #12379 ) ;
#23043 = CARTESIAN_POINT ( 'NONE',  ( -23.36965697125209473, -11.52193136556785547, 20.00001200000000523 ) ) ;
#23044 = CARTESIAN_POINT ( 'NONE',  ( 3.756430356250003655, -8.999999999999992895, 4.190624999385480720 ) ) ;
#23045 = CARTESIAN_POINT ( 'NONE',  ( 1.000000000000000000, 0.000000000000000000, 19.50000000000000000 ) ) ;
#23046 = CARTESIAN_POINT ( 'NONE',  ( -26.52310962334728828, 16.23990935651745460, -6.500000000000000000 ) ) ;
#23047 = CARTESIAN_POINT ( 'NONE',  ( 30.85476721088027929, 3.897863563849760737, -6.500000000000000000 ) ) ;
#23048 = DIRECTION ( 'NONE',  ( 0.000000000000000000, -0.000000000000000000, -1.000000000000000000 ) ) ;
#23049 = CARTESIAN_POINT ( 'NONE',  ( 3.735045420075836212E-15, -4.662447845253954171, 3.515624999385486227 ) ) ;
#23050 = EDGE_CURVE ( 'NONE', #5730, #17641, #14123, .T. ) ;
#23051 = CARTESIAN_POINT ( 'NONE',  ( -2.000000000000003997, -25.97500000000000142, 5.535898384862238508 ) ) ;
#23052 = ORIENTED_EDGE ( 'NONE', *, *, #16833, .F. ) ;
#23053 = EDGE_LOOP ( 'NONE', ( #24229, #24893, #21092 ) ) ;
#23054 = EDGE_CURVE ( 'NONE', #7170, #16822, #7976, .T. ) ;
#23055 = CIRCLE ( 'NONE', #2999, 4.000000000000000000 ) ;
#23056 = ORIENTED_EDGE ( 'NONE', *, *, #15178, .T. ) ;
#23057 = DIRECTION ( 'NONE',  ( 0.000000000000000000, 0.000000000000000000, -1.000000000000000000 ) ) ;
#23058 = EDGE_LOOP ( 'NONE', ( #22677, #25412, #12390, #23319 ) ) ;
#23059 = FACE_OUTER_BOUND ( 'NONE', #12589, .T. ) ;
#23060 = EDGE_CURVE ( 'NONE', #15870, #23630, #9229, .T. ) ;
#23061 = ORIENTED_EDGE ( 'NONE', *, *, #17070, .F. ) ;
#23062 = FACE_OUTER_BOUND ( 'NONE', #21449, .T. ) ;
#23063 = AXIS2_PLACEMENT_3D ( 'NONE', #11774, #12014, #2096 ) ;
#23064 = AXIS2_PLACEMENT_3D ( 'NONE', #812, #12583, #571 ) ;
#23065 = VERTEX_POINT ( 'NONE', #1849 ) ;
#23066 = EDGE_CURVE ( 'NONE', #17442, #4475, #23432, .T. ) ;
#23067 = DIRECTION ( 'NONE',  ( -0.000000000000000000, -0.000000000000000000, 1.000000000000000000 ) ) ;
#23068 = CARTESIAN_POINT ( 'NONE',  ( 3.752267015613588906E-15, 25.56250000000000000, 4.381197846482986158 ) ) ;
#23069 = CARTESIAN_POINT ( 'NONE',  ( 3.999999999999997335, -27.51250000000000284, 11.30940107675849404 ) ) ;
#23070 = AXIS2_PLACEMENT_3D ( 'NONE', #14054, #22152, #14563 ) ;
#23071 = DIRECTION ( 'NONE',  ( 0.000000000000000000, -0.000000000000000000, 1.000000000000000000 ) ) ;
#23072 = CARTESIAN_POINT ( 'NONE',  ( 18.19474136253732865, 18.19474136253726471, 12.99999999999999289 ) ) ;
#23073 = CARTESIAN_POINT ( 'NONE',  ( 17.90741546755112523, 20.56361284551042701, 5.746835883940462963 ) ) ;
#23074 = CARTESIAN_POINT ( 'NONE',  ( 18.83113746560522728, 18.83113746560514912, 12.99999999999999112 ) ) ;
#23075 = AXIS2_PLACEMENT_3D ( 'NONE', #10719, #20800, #18706 ) ;
#23076 = CARTESIAN_POINT ( 'NONE',  ( 4.000000000000003553, 26.38750000000000284, 6.690598923241489970 ) ) ;
#23077 = AXIS2_PLACEMENT_3D ( 'NONE', #23556, #13739, #8122 ) ;
#23078 = CARTESIAN_POINT ( 'NONE',  ( 19.76811771667562567, 17.11192033871618534, 12.25316411605952283 ) ) ;
#23079 = CARTESIAN_POINT ( 'NONE',  ( -0.7500000000000001110, 1.299038105676658450, 17.69999999999999929 ) ) ;
#23080 = VERTEX_POINT ( 'NONE', #15825 ) ;
#23081 = VERTEX_POINT ( 'NONE', #7 ) ;
#23082 = CARTESIAN_POINT ( 'NONE',  ( -3.999999999999996447, 27.00624999877096855, 11.30940107675849404 ) ) ;
#23083 = CARTESIAN_POINT ( 'NONE',  ( -1.878215178125004048, -27.46562499938548640, 5.746835883940462963 ) ) ;
#23084 = EDGE_CURVE ( 'NONE', #8796, #16116, #20912, .T. ) ;
#23085 = CARTESIAN_POINT ( 'NONE',  ( -1.999999999999998224, 27.10000000000000142, 12.46410161513774639 ) ) ;
#23086 = CARTESIAN_POINT ( 'NONE',  ( 1.878215178125004048, 27.57812499938548711, 5.746835883940462963 ) ) ;
#23087 = CARTESIAN_POINT ( 'NONE',  ( -17.87326343783906424, 25.45105997952945387, -2.750000000000000000 ) ) ;
#23088 = ORIENTED_EDGE ( 'NONE', *, *, #20248, .T. ) ;
#23089 = EDGE_CURVE ( 'NONE', #1087, #19275, #9811, .T. ) ;
#23090 = ORIENTED_EDGE ( 'NONE', *, *, #13575, .F. ) ;
#23091 = DIRECTION ( 'NONE',  ( 1.000000000000000000, 0.000000000000000000, 0.000000000000000000 ) ) ;
#23092 = CIRCLE ( 'NONE', #11807, 1.500000000000000222 ) ;
#23093 = DIRECTION ( 'NONE',  ( 0.000000000000000000, 0.000000000000000000, 1.000000000000000000 ) ) ;
#23094 = VERTEX_POINT ( 'NONE', #23798 ) ;
#23095 = EDGE_CURVE ( 'NONE', #23505, #19518, #7138, .T. ) ;
#23096 = CARTESIAN_POINT ( 'NONE',  ( 1.878215178124998497, -28.25312499938548427, 12.25316411605951927 ) ) ;
#23097 = DIRECTION ( 'NONE',  ( 1.000000000000000000, 0.000000000000000000, 0.000000000000000000 ) ) ;
#23098 = CARTESIAN_POINT ( 'NONE',  ( 3.756430356250002323, 25.62812499938548072, 6.831223922626973533 ) ) ;
#23099 = EDGE_CURVE ( 'NONE', #17369, #24372, #10307, .T. ) ;
#23100 = AXIS2_PLACEMENT_3D ( 'NONE', #207, #2293, #18245 ) ;
#23101 = DIRECTION ( 'NONE',  ( 0.9048270524660195768, -0.4257792915650726040, 0.000000000000000000 ) ) ;
#23102 = CARTESIAN_POINT ( 'NONE',  ( -3.999999999999999556, 25.18750000000000711, 6.690598923241487306 ) ) ;
#23103 = SHAPE_DEFINITION_REPRESENTATION ( #16121, #13517 ) ;
#23104 = DIRECTION ( 'NONE',  ( -0.000000000000000000, -1.000000000000000000, -0.000000000000000000 ) ) ;
#23105 = CARTESIAN_POINT ( 'NONE',  ( 29.72853858738278987, -9.133673601486577809, -6.500000000000000000 ) ) ;
#23106 = AXIS2_PLACEMENT_3D ( 'NONE', #6329, #12342, #12462 ) ;
#23107 = CARTESIAN_POINT ( 'NONE',  ( 3.756430356250002323, 27.35312499938547859, 11.16877607737301403 ) ) ;
#23108 = CARTESIAN_POINT ( 'NONE',  ( -1.999999999999998224, 27.04374999877097352, 12.46410161513774639 ) ) ;
#23109 = CARTESIAN_POINT ( 'NONE',  ( 15.03485793497900502, 20.69171218447132077, 11.30940107675849404 ) ) ;
#23110 = CARTESIAN_POINT ( 'NONE',  ( 19.20899765223631306, 19.20899765223624200, 4.662447845253954171 ) ) ;
#23111 = CARTESIAN_POINT ( 'NONE',  ( 19.98460540328483859, 19.98460540328476398, 4.999999999999992006 ) ) ;
#23112 = CARTESIAN_POINT ( 'NONE',  ( -1.878215178124998497, 28.14062499938548356, 12.25316411605951927 ) ) ;
#23113 = CYLINDRICAL_SURFACE ( 'NONE', #22509, 0.5000000000000004441 ) ;
#23114 = CARTESIAN_POINT ( 'NONE',  ( 22.34249210749660364, 17.03009735157778337, 8.999999999999992895 ) ) ;
#23115 = CARTESIAN_POINT ( 'NONE',  ( 21.64308941267829312, 20.12733988482615288, 4.999999999999997335 ) ) ;
#23116 = ORIENTED_EDGE ( 'NONE', *, *, #3296, .T. ) ;
#23117 = CARTESIAN_POINT ( 'NONE',  ( -1.999999999999995781, 26.44374999877096855, 5.535898384862237620 ) ) ;
#23118 = CARTESIAN_POINT ( 'NONE',  ( -1.999999999999995781, 29.14374999877096784, 5.535898384862237620 ) ) ;
#23119 = CARTESIAN_POINT ( 'NONE',  ( -3.735045420075836212E-15, -28.85312499938548569, 4.662447845253954171 ) ) ;
#23121 = VERTEX_POINT ( 'NONE', #6402 ) ;
#23120 = LINE ( 'NONE', #10682, #18365 ) ;
#23122 = CARTESIAN_POINT ( 'NONE',  ( 1.878215178125000939, 25.62812499938548783, 12.25316411605952283 ) ) ;
#23123 = EDGE_LOOP ( 'NONE', ( #12884, #20228, #25840, #9824 ) ) ;
#23124 = EDGE_CURVE ( 'NONE', #6672, #1492, #11309, .T. ) ;
#23125 = CARTESIAN_POINT ( 'NONE',  ( 3.756430356249997882, -28.55312499938548498, 11.16877607737301226 ) ) ;
#23126 = VERTEX_POINT ( 'NONE', #16213 ) ;
#23127 = ORIENTED_EDGE ( 'NONE', *, *, #16474, .T. ) ;
#23128 = DIRECTION ( 'NONE',  ( 0.000000000000000000, 0.000000000000000000, 1.000000000000000000 ) ) ;
#23129 = CARTESIAN_POINT ( 'NONE',  ( 3.756430356250004543, 28.89062499938549067, 6.831223922626973533 ) ) ;
#23130 = EDGE_CURVE ( 'NONE', #7738, #20939, #7981, .T. ) ;
#23131 = CIRCLE ( 'NONE', #21447, 0.4999999999999999445 ) ;
#23132 = CARTESIAN_POINT ( 'NONE',  ( 3.756430356250003211, -6.831223922626973533, 1.528124999385481964 ) ) ;
#23133 =( BOUNDED_CURVE ( )  B_SPLINE_CURVE ( 2, ( #2572, #8706, #494, #10396, #18652, #4798, #6491, #14739, #18394 ),
 .UNSPECIFIED., .F., .F. ) 
 B_SPLINE_CURVE_WITH_KNOTS ( ( 3, 2, 2, 2, 3 ),
 ( 0.7750000000000000222, 0.7833333333333333259, 0.8000000000000000444, 0.8166666666666666519, 0.8250000000000000666 ),
 .UNSPECIFIED. ) 
 CURVE ( )  GEOMETRIC_REPRESENTATION_ITEM ( )  RATIONAL_B_SPLINE_CURVE ( ( 0.9330127018922194093, 0.9330127018922194093, 1.000000000000000000, 0.8660254037844387076, 1.000000000000000000, 0.8660254037844387076, 1.000000000000000000, 0.9330127018922189652, 0.9330127018922194093 ) ) 
 REPRESENTATION_ITEM ( '' )  );
#23134 = CARTESIAN_POINT ( 'NONE',  ( 4.000000000000001776, 28.95624999877097494, 11.30940107675849760 ) ) ;
#23135 = LINE ( 'NONE', #1423, #24320 ) ;
#23136 =( BOUNDED_CURVE ( )  B_SPLINE_CURVE ( 2, ( #23175, #25384, #11013, #13504, #11523, #7471, #3548, #5256, #9317 ),
 .UNSPECIFIED., .F., .F. ) 
 B_SPLINE_CURVE_WITH_KNOTS ( ( 3, 2, 2, 2, 3 ),
 ( 0.1250000000000000000, 0.1333333333333333315, 0.1499999999999999944, 0.1666666666666666574, 0.1749999999999999889 ),
 .UNSPECIFIED. ) 
 CURVE ( )  GEOMETRIC_REPRESENTATION_ITEM ( )  RATIONAL_B_SPLINE_CURVE ( ( 0.9330127018922194093, 0.9330127018922194093, 1.000000000000000000, 0.8660254037844387076, 1.000000000000000000, 0.8660254037844387076, 1.000000000000000000, 0.9330127018922194093, 0.9330127018922194093 ) ) 
 REPRESENTATION_ITEM ( '' )  );
#23137 = CARTESIAN_POINT ( 'NONE',  ( 4.648177544792955347E-16, 28.93750000000000355, 12.99999999999999289 ) ) ;
#23138 = CARTESIAN_POINT ( 'NONE',  ( 4.000000000000003553, -8.999999999999992895, 0.9000000000000014655 ) ) ;
#23139 = CARTESIAN_POINT ( 'NONE',  ( -3.756430356249996105, 27.57812499938548356, 6.831223922626973533 ) ) ;
#23140 = CARTESIAN_POINT ( 'NONE',  ( 5.706339097770929847, 29.50000000000000000, 10.85410196624966517 ) ) ;
#23141 = CARTESIAN_POINT ( 'NONE',  ( -13.69242354489114177, 27.92360179968391165, -2.750000000000000000 ) ) ;
#23142 = CARTESIAN_POINT ( 'NONE',  ( 0.000000000000000000, 0.000000000000000000, 1.000000000000000000 ) ) ;
#23143 = CARTESIAN_POINT ( 'NONE',  ( -3.063240906311874401, -29.84319947910909931, 11.57226653943512851 ) ) ;
#23144 = CARTESIAN_POINT ( 'NONE',  ( -1.878215178125000939, -28.77812499938548640, 12.25316411605952283 ) ) ;
#23145 = CARTESIAN_POINT ( 'NONE',  ( 18.66319960507342302, 21.49162672981954003, 12.46410161513774639 ) ) ;
#23146 = LINE ( 'NONE', #22761, #23322 ) ;
#23147 = CARTESIAN_POINT ( 'NONE',  ( 3.834746474454188013E-15, 25.95624999877096428, 4.999999999999992006 ) ) ;
#23148 = CARTESIAN_POINT ( 'NONE',  ( 23.05168106668148553, 17.39482681718902768, 8.999999999999992895 ) ) ;
#23149 = ORIENTED_EDGE ( 'NONE', *, *, #17150, .T. ) ;
#23150 = DIRECTION ( 'NONE',  ( 1.000000000000000000, 0.000000000000000000, 0.000000000000000000 ) ) ;
#23152 = ORIENTED_EDGE ( 'NONE', *, *, #8977, .F. ) ;
#23151 = DIRECTION ( 'NONE',  ( 0.000000000000000000, 0.000000000000000000, 1.000000000000000000 ) ) ;
#23153 = EDGE_LOOP ( 'NONE', ( #20671, #23522, #7496, #16198 ) ) ;
#23154 = ORIENTED_EDGE ( 'NONE', *, *, #8020, .T. ) ;
#23155 = VERTEX_POINT ( 'NONE', #19989 ) ;
#23156 = ORIENTED_EDGE ( 'NONE', *, *, #16714, .T. ) ;
#23157 = ADVANCED_FACE ( 'NONE', ( #19865 ), #6017, .F. ) ;
#23158 = CARTESIAN_POINT ( 'NONE',  ( 5.840899737312978957, 34.50000000000000000, 10.37254881831474052 ) ) ;
#23159 = CARTESIAN_POINT ( 'NONE',  ( -1.999999999999995781, 29.14374999877096784, 5.535898384862237620 ) ) ;
#23160 = CARTESIAN_POINT ( 'NONE',  ( 0.000000000000000000, 0.000000000000000000, -6.500000000000000000 ) ) ;
#23161 = EDGE_CURVE ( 'NONE', #8256, #7798, #23967, .T. ) ;
#23162 = CARTESIAN_POINT ( 'NONE',  ( 3.756430356250004099, -6.831223922626973533, 4.340624999385483740 ) ) ;
#23163 = CARTESIAN_POINT ( 'NONE',  ( -1.999999999999998224, -12.46410161513774639, 2.493749998770968812 ) ) ;
#23164 = DIRECTION ( 'NONE',  ( 1.000000000000000000, 0.000000000000000000, 0.000000000000000000 ) ) ;
#23165 = CARTESIAN_POINT ( 'NONE',  ( 3.756430356250002323, 26.11562499938548498, 11.16877607737301226 ) ) ;
#23166 = EDGE_CURVE ( 'NONE', #11885, #13215, #2858, .T. ) ;
#23167 = CARTESIAN_POINT ( 'NONE',  ( 1.071796769724498999, 28.45134618820330275, 12.99999999999998757 ) ) ;
#23168 = CARTESIAN_POINT ( 'NONE',  ( 3.752267015613588906E-15, -4.381197846482986158, 0.5624999999999986677 ) ) ;
#23169 = DIRECTION ( 'NONE',  ( -0.6374239897486843054, 0.7705132427757935831, 0.000000000000000000 ) ) ;
#23170 = CARTESIAN_POINT ( 'NONE',  ( 3.469446951953614189E-15, 40.00000000000000000, 4.999999999999992006 ) ) ;
#23171 = CARTESIAN_POINT ( 'NONE',  ( 17.51415108564528467, 23.17100533513759331, 8.999999999999992895 ) ) ;
#23172 = CARTESIAN_POINT ( 'NONE',  ( 1.999999999999998224, -27.94374999877096855, 12.46410161513774639 ) ) ;
#23173 = CARTESIAN_POINT ( 'NONE',  ( -3.999999999999982681, -6.690598923241479312, 0.5812499987709673910 ) ) ;
#23174 = CARTESIAN_POINT ( 'NONE',  ( -3.999999999999996447, 25.22500000000000497, 8.999999999999992895 ) ) ;
#23175 = CARTESIAN_POINT ( 'NONE',  ( 3.834746474454188013E-15, 25.56250000000000000, 4.999999999999992006 ) ) ;
#23176 = ORIENTED_EDGE ( 'NONE', *, *, #9394, .T. ) ;
#23177 = VERTEX_POINT ( 'NONE', #12805 ) ;
#23178 = EDGE_LOOP ( 'NONE', ( #12268, #17903, #2603, #21537 ) ) ;
#23179 = CARTESIAN_POINT ( 'NONE',  ( -3.469446951953614189E-15, -30.00000000000000355, 8.999999999999992895 ) ) ;
#23180 = ORIENTED_EDGE ( 'NONE', *, *, #10022, .F. ) ;
#23181 = DIRECTION ( 'NONE',  ( 0.000000000000000000, 0.000000000000000000, 1.000000000000000000 ) ) ;
#23182 = ORIENTED_EDGE ( 'NONE', *, *, #20091, .F. ) ;
#23183 = CARTESIAN_POINT ( 'NONE',  ( 1.859271017917182139E-15, 26.68750000000000000, 12.99999999999999289 ) ) ;
#23184 = EDGE_LOOP ( 'NONE', ( #18753, #3553, #24938, #15271 ) ) ;
#23185 = CARTESIAN_POINT ( 'NONE',  ( -3.999999999999997335, 27.51250000000000284, 11.30940107675849404 ) ) ;
#23186 = DIRECTION ( 'NONE',  ( 0.000000000000000000, 0.000000000000000000, 1.000000000000000000 ) ) ;
#23187 = EDGE_CURVE ( 'NONE', #15991, #20076, #655, .T. ) ;
#23188 = CYLINDRICAL_SURFACE ( 'NONE', #18014, 0.5000000000000004441 ) ;
#23189 = CARTESIAN_POINT ( 'NONE',  ( 3.469446951953614189E-15, 40.00000000000000000, 4.999999999999992006 ) ) ;
#23190 = CARTESIAN_POINT ( 'NONE',  ( 21.81216202160668871, 16.49976726568787200, 6.831223922626973533 ) ) ;
#23191 = CARTESIAN_POINT ( 'NONE',  ( 3.469446951953614189E-15, 31.50000000000000000, 8.999999999999992895 ) ) ;
#23192 = EDGE_CURVE ( 'NONE', #17006, #13301, #14778, .T. ) ;
#23193 = CARTESIAN_POINT ( 'NONE',  ( -1.999999999999998224, 26.64999999999999858, 12.46410161513774639 ) ) ;
#23194 = CARTESIAN_POINT ( 'NONE',  ( 17.27101936448323016, 19.92721674244253549, 5.746835883940462963 ) ) ;
#23195 = CARTESIAN_POINT ( 'NONE',  ( -4.393401135980685268, 30.78811501957149588, -2.750000000000000000 ) ) ;
#23196 = ORIENTED_EDGE ( 'NONE', *, *, #14305, .F. ) ;
#23197 = ORIENTED_EDGE ( 'NONE', *, *, #6435, .T. ) ;
#23198 = CARTESIAN_POINT ( 'NONE',  ( 4.000000000000002665, 27.23124999877097352, 6.690598923241489970 ) ) ;
#23199 = SHAPE_REPRESENTATION ( 'bezel', ( #21036 ), #23570 ) ;
#23200 = CARTESIAN_POINT ( 'NONE',  ( -3.756430356250002323, -29.60312499938548569, 11.16877607737301403 ) ) ;
#23201 = EDGE_LOOP ( 'NONE', ( #4734, #2626, #20607, #17105 ) ) ;
#23202 = FACE_OUTER_BOUND ( 'NONE', #24204, .T. ) ;
#23203 = CARTESIAN_POINT ( 'NONE',  ( 3.756430356250003655, 27.95312499938548711, 8.999999999999992895 ) ) ;
#23204 = CARTESIAN_POINT ( 'NONE',  ( -31.09598070739550835, -0.4999838450256507416, 1.000000000000000000 ) ) ;
#23205 = ORIENTED_EDGE ( 'NONE', *, *, #15211, .T. ) ;
#23206 = ORIENTED_EDGE ( 'NONE', *, *, #1215, .F. ) ;
#23207 = DIRECTION ( 'NONE',  ( 0.000000000000000000, 0.000000000000000000, -1.000000000000000000 ) ) ;
#23208 = CARTESIAN_POINT ( 'NONE',  ( 20.20656826142273843, 23.64116323484239146, 1.000000000000000000 ) ) ;
#23209 = VERTEX_POINT ( 'NONE', #18685 ) ;
#23210 = EDGE_CURVE ( 'NONE', #24890, #19876, #22123, .T. ) ;
#23211 = CARTESIAN_POINT ( 'NONE',  ( 3.756430356249996994, -28.17812499938548498, 8.999999999999992895 ) ) ;
#23212 = CARTESIAN_POINT ( 'NONE',  ( -3.756430356249998326, 29.45312499938549422, 11.16877607737301226 ) ) ;
#23213 = CARTESIAN_POINT ( 'NONE',  ( 1.878215178124998275, 25.51562499938548711, 12.25316411605952283 ) ) ;
#23214 = CIRCLE ( 'NONE', #11932, 0.5000000000000005551 ) ;
#23215 = DIRECTION ( 'NONE',  ( 0.000000000000000000, 0.000000000000000000, 1.000000000000000000 ) ) ;
#23216 = CARTESIAN_POINT ( 'NONE',  ( -1.878215178124998275, 29.49062499938548854, 12.25316411605951927 ) ) ;
#23217 = ADVANCED_FACE ( 'NONE', ( #16876 ), #9012, .T. ) ;
#23218 = CARTESIAN_POINT ( 'NONE',  ( 0.5000000000000000000, -0.8660254037844387076, 20.00000000000000000 ) ) ;
#23219 = APPLICATION_PROTOCOL_DEFINITION ( 'draft international standard', 'automotive_design', 1998, #17136 ) ;
#23220 = EDGE_CURVE ( 'NONE', #24134, #18284, #1583, .T. ) ;
#23221 = DIRECTION ( 'NONE',  ( 0.000000000000000000, 0.000000000000000000, -1.000000000000000000 ) ) ;
#23222 = DIRECTION ( 'NONE',  ( 0.000000000000000000, 0.000000000000000000, 1.000000000000000000 ) ) ;
#23223 = CARTESIAN_POINT ( 'NONE',  ( 3.756430356250003655, 26.04062499938548569, 8.999999999999992895 ) ) ;
#23224 = CARTESIAN_POINT ( 'NONE',  ( -3.872397317694597163, -29.74907003676636563, 7.964378325765101962 ) ) ;
#23225 = CARTESIAN_POINT ( 'NONE',  ( 19.52492222951535439, 22.18111960747465261, 12.25316411605951927 ) ) ;
#23226 = CARTESIAN_POINT ( 'NONE',  ( 17.37708538166121386, 20.03328275962052274, 12.25316411605951927 ) ) ;
#23227 = EDGE_CURVE ( 'NONE', #8694, #15051, #15913, .T. ) ;
#23228 = CARTESIAN_POINT ( 'NONE',  ( 16.21484237521500660, 21.87169662470731168, 6.690598923241487306 ) ) ;
#23229 = CARTESIAN_POINT ( 'NONE',  ( -1.878215178124995832, 28.44062499938548427, 5.746835883940462963 ) ) ;
#23230 = CYLINDRICAL_SURFACE ( 'NONE', #17507, 4.000000000000000000 ) ;
#23231 = CARTESIAN_POINT ( 'NONE',  ( 19.76584424242071947, 19.76584424242064486, 4.662447845253954171 ) ) ;
#23232 = CARTESIAN_POINT ( 'NONE',  ( 19.94483064597403654, 19.94483064597395838, 4.999999999999992006 ) ) ;
#23233 = VERTEX_POINT ( 'NONE', #24564 ) ;
#23234 = CYLINDRICAL_SURFACE ( 'NONE', #25553, 0.5000000000000000000 ) ;
#23235 = CARTESIAN_POINT ( 'NONE',  ( 3.756430356250002323, 26.56562499938548427, 11.16877607737301226 ) ) ;
#23236 = CARTESIAN_POINT ( 'NONE',  ( 3.756430356249996994, -28.96562499938548285, 8.999999999999992895 ) ) ;
#23238 = ORIENTED_EDGE ( 'NONE', *, *, #25751, .F. ) ;
#23237 = CARTESIAN_POINT ( 'NONE',  ( -3.999999999999997335, 25.65624999877097068, 11.30940107675849404 ) ) ;
#23239 = CARTESIAN_POINT ( 'NONE',  ( 3.756430356250003211, 25.74062499938548498, 6.831223922626973533 ) ) ;
#23240 = ORIENTED_EDGE ( 'NONE', *, *, #1697, .F. ) ;
#23241 = CARTESIAN_POINT ( 'NONE',  ( -3.735045420075836212E-15, -27.95312499938548001, 4.662447845253954171 ) ) ;
#23242 = ORIENTED_EDGE ( 'NONE', *, *, #20926, .F. ) ;
#23243 = ORIENTED_EDGE ( 'NONE', *, *, #22473, .T. ) ;
#23244 = SURFACE_STYLE_FILL_AREA ( #25220 ) ;
#23245 = CARTESIAN_POINT ( 'NONE',  ( 2.003086131649545506E-15, 27.39062499938549067, 13.33755215474602984 ) ) ;
#23246 = CARTESIAN_POINT ( 'NONE',  ( 3.756430356250003655, -8.999999999999992895, 1.940624999385482496 ) ) ;
#23247 = CARTESIAN_POINT ( 'NONE',  ( 3.756430356250003655, -8.999999999999992895, 4.753124999385485161 ) ) ;
#23248 = FILL_AREA_STYLE ('',( #11348 ) ) ;
#23249 = LINE ( 'NONE', #7686, #12203 ) ;
#23250 = CARTESIAN_POINT ( 'NONE',  ( 0.000000000000000000, 0.000000000000000000, 19.50000000000000000 ) ) ;
#23251 = DIRECTION ( 'NONE',  ( -0.000000000000000000, 0.000000000000000000, 1.000000000000000000 ) ) ;
#23252 = PRODUCT_DEFINITION_CONTEXT ( 'detailed design', #15450, 'design' ) ;
#23253 = CARTESIAN_POINT ( 'NONE',  ( 14.98253926456337837, 27.25313774936414291, 1.000000000000000000 ) ) ;
#23254 = CARTESIAN_POINT ( 'NONE',  ( 3.469446951953614189E-15, 35.50000000000000711, 4.999999999999992006 ) ) ;
#23255 = LINE ( 'NONE', #20920, #13057 ) ;
#23256 = EDGE_CURVE ( 'NONE', #19772, #21027, #3790, .T. ) ;
#23257 = CARTESIAN_POINT ( 'NONE',  ( -25.99307600111999150, -0.5999999999999998668, 20.00001200000000168 ) ) ;
#23258 = CARTESIAN_POINT ( 'NONE',  ( -2.672651547586948120E-15, -28.29062499938548569, 13.33755215474602984 ) ) ;
#23259 = CARTESIAN_POINT ( 'NONE',  ( 0.000000000000000000, 0.000000000000000000, 1.000000000000000000 ) ) ;
#23260 = EDGE_CURVE ( 'NONE', #19181, #3646, #4252, .T. ) ;
#23261 = DIRECTION ( 'NONE',  ( 1.000000000000000000, 0.000000000000000000, 0.000000000000000000 ) ) ;
#23262 = CARTESIAN_POINT ( 'NONE',  ( 4.000000000000003553, -8.999999999999992895, 4.500000000000000888 ) ) ;
#23263 = CARTESIAN_POINT ( 'NONE',  ( -2.451530025008687996, 31.00322564728517349, -6.500000000000000000 ) ) ;
#23264 = ORIENTED_EDGE ( 'NONE', *, *, #7267, .F. ) ;
#23265 = CARTESIAN_POINT ( 'NONE',  ( -1.878215178124996498, 29.45312499938548711, 5.746835883940462963 ) ) ;
#23266 = CARTESIAN_POINT ( 'NONE',  ( 0.000000000000000000, 0.000000000000000000, -6.500000000000000000 ) ) ;
#23268 = ORIENTED_EDGE ( 'NONE', *, *, #8390, .F. ) ;
#23267 = DIRECTION ( 'NONE',  ( -0.000000000000000000, -1.000000000000000000, -0.000000000000000000 ) ) ;
#23269 = EDGE_CURVE ( 'NONE', #24827, #21865, #4952, .T. ) ;
#23270 = ORIENTED_EDGE ( 'NONE', *, *, #14865, .F. ) ;
#23271 = EDGE_CURVE ( 'NONE', #21953, #3228, #7558, .T. ) ;
#23272 = ORIENTED_EDGE ( 'NONE', *, *, #21964, .T. ) ;
#23273 = ORIENTED_EDGE ( 'NONE', *, *, #15842, .F. ) ;
#23274 = ORIENTED_EDGE ( 'NONE', *, *, #7451, .F. ) ;
#23275 = DIRECTION ( 'NONE',  ( 0.000000000000000000, 0.000000000000000000, 1.000000000000000000 ) ) ;
#23276 =( BOUNDED_CURVE ( )  B_SPLINE_CURVE ( 2, ( #15830, #23803, #11901, #7986, #2864, #22757, #24327, #10703, #6921 ),
 .UNSPECIFIED., .F., .F. ) 
 B_SPLINE_CURVE_WITH_KNOTS ( ( 3, 2, 2, 2, 3 ),
 ( 0.07500000000000001110, 0.08333333333333332871, 0.1000000000000000056, 0.1166666666666666685, 0.1250000000000000000 ),
 .UNSPECIFIED. ) 
 CURVE ( )  GEOMETRIC_REPRESENTATION_ITEM ( )  RATIONAL_B_SPLINE_CURVE ( ( 0.9330127018922192983, 0.9330127018922194093, 1.000000000000000000, 0.8660254037844387076, 1.000000000000000000, 0.8660254037844387076, 1.000000000000000000, 0.9330127018922194093, 0.9330127018922194093 ) ) 
 REPRESENTATION_ITEM ( '' )  );
#23277 = DIRECTION ( 'NONE',  ( 1.000000000000000000, 0.000000000000000000, 0.000000000000000000 ) ) ;
#23278 = DIRECTION ( 'NONE',  ( 1.000000000000000000, 0.000000000000000000, 0.000000000000000000 ) ) ;
#23279 =( BOUNDED_CURVE ( )  B_SPLINE_CURVE ( 2, ( #9374, #11183, #17355, #23228, #25205, #7283, #15379, #21140, #15647 ),
 .UNSPECIFIED., .F., .F. ) 
 B_SPLINE_CURVE_WITH_KNOTS ( ( 3, 2, 2, 2, 3 ),
 ( 0.3250000000000000111, 0.3333333333333333148, 0.3499999999999999778, 0.3666666666666666408, 0.3750000000000000000 ),
 .UNSPECIFIED. ) 
 CURVE ( )  GEOMETRIC_REPRESENTATION_ITEM ( )  RATIONAL_B_SPLINE_CURVE ( ( 0.9330127018922194093, 0.9330127018922196314, 1.000000000000000000, 0.8660254037844387076, 1.000000000000000000, 0.8660254037844387076, 1.000000000000000000, 0.9330127018922194093, 0.9330127018922194093 ) ) 
 REPRESENTATION_ITEM ( '' )  );
#23280 = CARTESIAN_POINT ( 'NONE',  ( 3.756430356250003655, -8.999999999999992895, 0.5906249993854819635 ) ) ;
#23281 = CARTESIAN_POINT ( 'NONE',  ( 4.000000000000001776, -11.30940107675849760, 2.606249998770964194 ) ) ;
#23282 = CARTESIAN_POINT ( 'NONE',  ( 3.756430356250003655, 25.25312499938548427, 8.999999999999992895 ) ) ;
#23283 = CARTESIAN_POINT ( 'NONE',  ( 1.453535542772610212, 31.06601413805602263, -2.750000000000000000 ) ) ;
#23284 = LINE ( 'NONE', #21465, #25149 ) ;
#23285 = CARTESIAN_POINT ( 'NONE',  ( 4.000000000000003553, -8.999999999999992895, 0.9000000000000014655 ) ) ;
#23286 = DIRECTION ( 'NONE',  ( -0.000000000000000000, -0.000000000000000000, 1.000000000000000000 ) ) ;
#23287 = PLANE ( 'NONE',  #9540 ) ;
#23288 = CYLINDRICAL_SURFACE ( 'NONE', #24717, 31.10000000000000142 ) ;
#23289 = CARTESIAN_POINT ( 'NONE',  ( -4.000000000000001776, -27.60624999877096641, 11.30940107675849760 ) ) ;
#23290 = DIRECTION ( 'NONE',  ( -0.7071067811865487940, -0.7071067811865463515, 0.000000000000000000 ) ) ;
#23291 = EDGE_CURVE ( 'NONE', #4422, #7506, #8504, .T. ) ;
#23292 = DIRECTION ( 'NONE',  ( 0.000000000000000000, 0.000000000000000000, 1.000000000000000000 ) ) ;
#23293 = AXIS2_PLACEMENT_3D ( 'NONE', #5667, #1884, #9846 ) ;
#23294 = CARTESIAN_POINT ( 'NONE',  ( 5.827558883616049457, 30.54913349766221842, 1.000000000000000000 ) ) ;
#23295 = CARTESIAN_POINT ( 'NONE',  ( -2.000000000000000888, -25.82499999999999929, 12.46410161513774817 ) ) ;
#23296 = VERTEX_POINT ( 'NONE', #4560 ) ;
#23297 = DIRECTION ( 'NONE',  ( -0.000000000000000000, -0.000000000000000000, -1.000000000000000000 ) ) ;
#23298 = ORIENTED_EDGE ( 'NONE', *, *, #2160, .T. ) ;
#23299 = ORIENTED_EDGE ( 'NONE', *, *, #809, .F. ) ;
#23300 = FACE_BOUND ( 'NONE', #12097, .T. ) ;
#23301 = ORIENTED_EDGE ( 'NONE', *, *, #21226, .T. ) ;
#23302 = CARTESIAN_POINT ( 'NONE',  ( -3.756430356250004099, -27.09062499938548285, 6.831223922626973533 ) ) ;
#23303 = ORIENTED_EDGE ( 'NONE', *, *, #19537, .F. ) ;
#23304 = CARTESIAN_POINT ( 'NONE',  ( 27.09999999999999787, -0.5999999999999998668, 19.59999999999999787 ) ) ;
#23305 = EDGE_CURVE ( 'NONE', #19496, #15395, #6936, .T. ) ;
#23306 = ORIENTED_EDGE ( 'NONE', *, *, #24765, .F. ) ;
#23307 = CARTESIAN_POINT ( 'NONE',  ( 4.000000000000003553, 28.18750000000000000, 6.690598923241489970 ) ) ;
#23308 = DIRECTION ( 'NONE',  ( 0.000000000000000000, 0.000000000000000000, 1.000000000000000000 ) ) ;
#23309 = VECTOR ( 'NONE', #3937, 1000.000000000000000 ) ;
#23310 = LINE ( 'NONE', #11415, #15511 ) ;
#23311 = LINE ( 'NONE', #19127, #5412 ) ;
#23312 = CARTESIAN_POINT ( 'NONE',  ( 20.75150184982686596, 15.43910709390805280, 8.999999999999992895 ) ) ;
#23313 = CARTESIAN_POINT ( 'NONE',  ( 14.54246377227358877, 27.49048467073853175, -6.500000000000000000 ) ) ;
#23314 = VECTOR ( 'NONE', #5636, 1000.000000000000000 ) ;
#23315 = CARTESIAN_POINT ( 'NONE',  ( 4.000000000000001776, 26.31250000000000000, 11.30940107675849760 ) ) ;
#23316 = CARTESIAN_POINT ( 'NONE',  ( 19.68629472953723436, 19.68629472953716686, 13.33755215474603162 ) ) ;
#23317 = CARTESIAN_POINT ( 'NONE',  ( 31.03863125411924173, -1.952785157361756951, -6.500000000000000000 ) ) ;
#23318 = ORIENTED_EDGE ( 'NONE', *, *, #2378, .F. ) ;
#23319 = ORIENTED_EDGE ( 'NONE', *, *, #7863, .T. ) ;
#23320 = CARTESIAN_POINT ( 'NONE',  ( 2.000000000000000000, 27.11874999877097281, 12.46410161513774817 ) ) ;
#23321 = CARTESIAN_POINT ( 'NONE',  ( -3.756430356250002323, -29.15312499938548640, 11.16877607737301403 ) ) ;
#23323 = ORIENTED_EDGE ( 'NONE', *, *, #5924, .F. ) ;
#23322 = VECTOR ( 'NONE', #23261, 1000.000000000000000 ) ;
#23324 = DIRECTION ( 'NONE',  ( 0.000000000000000000, 0.000000000000000000, 1.000000000000000000 ) ) ;
#23325 = ADVANCED_FACE ( 'NONE', ( #1424 ), #11212, .T. ) ;
#23326 = CIRCLE ( 'NONE', #12044, 31.10000000000000142 ) ;
#23327 = CARTESIAN_POINT ( 'NONE',  ( 2.672651547586948120E-15, 28.74062499938548498, 13.33755215474602984 ) ) ;
#23328 = CARTESIAN_POINT ( 'NONE',  ( 0.000000000000000000, 0.000000000000000000, 20.00000000000000000 ) ) ;
#23329 = EDGE_LOOP ( 'NONE', ( #25551, #1350, #11617, #18292 ) ) ;
#23330 = ORIENTED_EDGE ( 'NONE', *, *, #4430, .T. ) ;
#23331 = DIRECTION ( 'NONE',  ( 0.000000000000000000, -0.000000000000000000, -1.000000000000000000 ) ) ;
#23332 = LINE ( 'NONE', #13656, #6469 ) ;
#23333 = AXIS2_PLACEMENT_3D ( 'NONE', #6470, #8176, #2679 ) ;
#23334 = ORIENTED_EDGE ( 'NONE', *, *, #21042, .F. ) ;
#23335 = CARTESIAN_POINT ( 'NONE',  ( 3.756430356249997438, -28.66562499938548569, 11.16877607737301048 ) ) ;
#23336 = CARTESIAN_POINT ( 'NONE',  ( 25.45105997952913057, -17.87326343783952254, -2.750000000000000000 ) ) ;
#23337 = CARTESIAN_POINT ( 'NONE',  ( 8.012344526598182026E-15, 28.85312499938549280, 4.662447845253954171 ) ) ;
#23338 = CARTESIAN_POINT ( 'NONE',  ( 13.24173596767378847, 28.14012133169319796, -6.500000000000000000 ) ) ;
#23339 = CARTESIAN_POINT ( 'NONE',  ( -3.999999999999999556, 25.26250000000000284, 11.30940107675849404 ) ) ;
#23340 = AXIS2_PLACEMENT_3D ( 'NONE', #24815, #4925, #20886 ) ;
#23341 = VECTOR ( 'NONE', #7493, 1000.000000000000114 ) ;
#23342 = CARTESIAN_POINT ( 'NONE',  ( 21.21320343559646915, 21.21320343559638744, 12.99999999999999289 ) ) ;
#23343 = SHAPE_REPRESENTATION ( 'contact point', ( #21036 ), #2676 ) ;
#23344 = VECTOR ( 'NONE', #18382, 1000.000000000000000 ) ;
#23345 = DIRECTION ( 'NONE',  ( 0.000000000000000000, 0.000000000000000000, 1.000000000000000000 ) ) ;
#23346 = CARTESIAN_POINT ( 'NONE',  ( 3.735045420075836212E-15, 26.15312499938548285, 4.662447845253954171 ) ) ;
#23347 = VECTOR ( 'NONE', #9524, 1000.000000000000000 ) ;
#23348 = CARTESIAN_POINT ( 'NONE',  ( 8.000000000000000000, 10.00000000000000000, 15.00000000000000178 ) ) ;
#23349 = CARTESIAN_POINT ( 'NONE',  ( 19.41885621233737069, 22.07505359029666536, 5.746835883940462963 ) ) ;
#23350 = CARTESIAN_POINT ( 'NONE',  ( 18.01348148472910893, 20.66967886268841426, 12.25316411605951927 ) ) ;
#23351 = DIRECTION ( 'NONE',  ( 0.000000000000000000, 0.000000000000000000, -1.000000000000000000 ) ) ;
#23352 = CARTESIAN_POINT ( 'NONE',  ( -3.756430356249995661, 29.37812499938548427, 6.831223922626973533 ) ) ;
#23353 = CARTESIAN_POINT ( 'NONE',  ( 22.58562062835815354, 19.74684143318851781, 5.530155478426870275 ) ) ;
#23354 = EDGE_CURVE ( 'NONE', #22067, #17688, #14256, .T. ) ;
#23355 = CARTESIAN_POINT ( 'NONE',  ( 18.65215106205190310, 18.65215106205183915, 13.33755215474603162 ) ) ;
#23356 = CARTESIAN_POINT ( 'NONE',  ( -5.706339097770898761, 31.50000000000000000, 10.85410196624973800 ) ) ;
#23357 = VERTEX_POINT ( 'NONE', #13460 ) ;
#23358 = FACE_OUTER_BOUND ( 'NONE', #13946, .T. ) ;
#23359 = CARTESIAN_POINT ( 'NONE',  ( -3.756430356249997882, 25.51562499938548356, 11.16877607737301226 ) ) ;
#23360 = CARTESIAN_POINT ( 'NONE',  ( -3.735045420075836212E-15, -28.40312499938548640, 4.662447845253954171 ) ) ;
#23361 = B_SPLINE_CURVE_WITH_KNOTS ( 'NONE', 3,
 ( #18866, #8932, #13112, #19368 ),
 .UNSPECIFIED., .F., .F.,
 ( 4, 4 ),
 ( 2.789812634830972505E-07, 0.0001914289244202972522 ),
 .UNSPECIFIED. ) ;
#23363 = ORIENTED_EDGE ( 'NONE', *, *, #24006, .T. ) ;
#23362 = CARTESIAN_POINT ( 'NONE',  ( 24.27856662945499266, 19.43607991388990186, 1.000000000000000000 ) ) ;
#23364 = DIRECTION ( 'NONE',  ( -0.000000000000000000, -1.000000000000000000, -0.000000000000000000 ) ) ;
#23365 = CIRCLE ( 'NONE', #17527, 0.4999999999999983902 ) ;
#23366 = EDGE_CURVE ( 'NONE', #23357, #7134, #13194, .T. ) ;
#23367 = CIRCLE ( 'NONE', #12083, 0.5000000000000017764 ) ;
#23368 = LINE ( 'NONE', #19439, #15484 ) ;
#23369 = CARTESIAN_POINT ( 'NONE',  ( 3.756430356249996994, -27.61562499938548143, 8.999999999999992895 ) ) ;
#23370 = EDGE_LOOP ( 'NONE', ( #12557, #10987, #9861, #11933 ) ) ;
#23371 = ORIENTED_EDGE ( 'NONE', *, *, #15340, .F. ) ;
#23372 = EDGE_CURVE ( 'NONE', #12921, #12737, #47, .T. ) ;
#23373 = CARTESIAN_POINT ( 'NONE',  ( 0.000000000000000000, 0.000000000000000000, -6.500000000000000000 ) ) ;
#23374 = CARTESIAN_POINT ( 'NONE',  ( -3.756430356249996105, 25.77812499938548640, 6.831223922626973533 ) ) ;
#23375 = AXIS2_PLACEMENT_3D ( 'NONE', #3444, #25541, #1748 ) ;
#23376 = CARTESIAN_POINT ( 'NONE',  ( 1.878215178125004048, -5.746835883940462963, 0.6656249993854841396 ) ) ;
#23377 = ADVANCED_FACE ( 'NONE', ( #15168 ), #9272, .T. ) ;
#23378 = VECTOR ( 'NONE', #20669, 1000.000000000000000 ) ;
#23379 = CARTESIAN_POINT ( 'NONE',  ( -1.878215178124995832, -5.746835883940462963, 3.553124999385485427 ) ) ;
#23380 = DIRECTION ( 'NONE',  ( 1.000000000000000000, 0.000000000000000000, 0.000000000000000000 ) ) ;
#23381 = CIRCLE ( 'NONE', #14207, 1.000000000000000000 ) ;
#23382 = CARTESIAN_POINT ( 'NONE',  ( -9.296355089585910693E-16, 26.91250000000000497, 4.999999999999991118 ) ) ;
#23383 = DIRECTION ( 'NONE',  ( -0.8660254037844397068, -0.4999999999999983347, 0.000000000000000000 ) ) ;
#23384 =( BOUNDED_CURVE ( )  B_SPLINE_CURVE ( 2, ( #14457, #17996, #4500, #2548, #10518, #24120, #8057, #18515, #602 ),
 .UNSPECIFIED., .F., .T. ) 
 B_SPLINE_CURVE_WITH_KNOTS ( ( 3, 2, 2, 2, 3 ),
 ( 0.8250000000000000666, 0.8333333333333333703, 0.8499999999999999778, 0.8666666666666666963, 0.8750000000000000000 ),
 .UNSPECIFIED. ) 
 CURVE ( )  GEOMETRIC_REPRESENTATION_ITEM ( )  RATIONAL_B_SPLINE_CURVE ( ( 0.9330127018922194093, 0.9330127018922198534, 1.000000000000000000, 0.8660254037844387076, 1.000000000000000000, 0.8660254037844387076, 1.000000000000000000, 0.9330127018922194093, 0.9330127018922194093 ) ) 
 REPRESENTATION_ITEM ( '' )  );
#23385 = CARTESIAN_POINT ( 'NONE',  ( 1.859271017917182139E-15, 26.68750000000000000, 12.99999999999999289 ) ) ;
#23386 = CARTESIAN_POINT ( 'NONE',  ( 3.834746474454188013E-15, 25.95624999877096428, 4.999999999999992006 ) ) ;
#23387 = CYLINDRICAL_SURFACE ( 'NONE', #12902, 31.10000000000000142 ) ;
#23388 = CARTESIAN_POINT ( 'NONE',  ( 19.95366948073886348, 17.12524235599260791, 12.46410161513774817 ) ) ;
#23389 = EDGE_LOOP ( 'NONE', ( #221, #6295, #5964, #1531 ) ) ;
#23390 = CARTESIAN_POINT ( 'NONE',  ( -2.610164000359269210, -29.83019057377770622, 12.11182326528050623 ) ) ;
#23391 = CARTESIAN_POINT ( 'NONE',  ( 1.500000000000001776, -7.499999999999993783, 4.999999999999993783 ) ) ;
#23392 = CARTESIAN_POINT ( 'NONE',  ( 2.672651547586948120E-15, 28.29062499938548569, 13.33755215474602984 ) ) ;
#23393 = CARTESIAN_POINT ( 'NONE',  ( 3.878215178125003604, -8.999999999999992895, 4.823437499078226942 ) ) ;
#23394 = CARTESIAN_POINT ( 'NONE',  ( -3.999999999999936051, -11.30940107675852779, 4.312500000000001776 ) ) ;
#23395 = CARTESIAN_POINT ( 'NONE',  ( -4.000000000000003553, -28.60000000000000142, 8.999999999999992895 ) ) ;
#23396 = VERTEX_POINT ( 'NONE', #11093 ) ;
#23397 = CARTESIAN_POINT ( 'NONE',  ( -1.878215178124999829, 29.15312499938549351, 12.25316411605951927 ) ) ;
#23398 = CARTESIAN_POINT ( 'NONE',  ( -5.706339097770933400, 38.63519838069944967, 7.645898033750358813 ) ) ;
#23400 = EDGE_LOOP ( 'NONE', ( #13484, #24260, #16950, #18700 ) ) ;
#23399 = CARTESIAN_POINT ( 'NONE',  ( 1.487416814333745711E-14, 28.43124999877096926, 12.99999999999999289 ) ) ;
#23401 = ORIENTED_EDGE ( 'NONE', *, *, #16311, .F. ) ;
#23402 = VECTOR ( 'NONE', #3075, 1000.000000000000000 ) ;
#23403 = ORIENTED_EDGE ( 'NONE', *, *, #18173, .F. ) ;
#23404 = ORIENTED_EDGE ( 'NONE', *, *, #14434, .T. ) ;
#23405 = ORIENTED_EDGE ( 'NONE', *, *, #12831, .T. ) ;
#23406 = CARTESIAN_POINT ( 'NONE',  ( 25.16042852506090810, 18.28012134629586072, -6.500000000000000000 ) ) ;
#23407=STYLED_ITEM('',(#25907),#14010);
#23408 = CARTESIAN_POINT ( 'NONE',  ( -1.071796769724488563, 29.31115380933863790, 12.99999999999999289 ) ) ;
#23409 = AXIS2_PLACEMENT_3D ( 'NONE', #10892, #1222, #21367 ) ;
#23410 = EDGE_CURVE ( 'NONE', #19215, #930, #19767, .T. ) ;
#23411 = CARTESIAN_POINT ( 'NONE',  ( -9.610428525060479288, 29.57785765677940404, -6.500000000000000000 ) ) ;
#23412 = ADVANCED_FACE ( 'NONE', ( #3238 ), #19193, .F. ) ;
#23413 = CARTESIAN_POINT ( 'NONE',  ( -3.756430356249997882, -11.16877607737301226, 3.553124999385482763 ) ) ;
#23414 = CARTESIAN_POINT ( 'NONE',  ( -3.999999999999996447, -8.999999999999992895, 1.518749998770968501 ) ) ;
#23415 = CARTESIAN_POINT ( 'NONE',  ( -1.878215178124998497, 27.35312499938548569, 12.25316411605951927 ) ) ;
#23416 = DIRECTION ( 'NONE',  ( 0.000000000000000000, 1.000000000000000000, 0.000000000000000000 ) ) ;
#23417 = DIRECTION ( 'NONE',  ( 0.000000000000000000, 0.000000000000000000, -1.000000000000000000 ) ) ;
#23418 = AXIS2_PLACEMENT_3D ( 'NONE', #20426, #8160, #10495 ) ;
#23419 = CARTESIAN_POINT ( 'NONE',  ( 4.000000000000001776, -11.30940107675849760, 2.212499999999997691 ) ) ;
#23420 = CARTESIAN_POINT ( 'NONE',  ( -5.577813053751546416E-15, -25.73124999877097352, 12.99999999999999289 ) ) ;
#23421 = DIRECTION ( 'NONE',  ( 1.000000000000000000, 0.000000000000000000, 0.000000000000000000 ) ) ;
#23422 = CYLINDRICAL_SURFACE ( 'NONE', #18062, 31.10000000000000142 ) ;
#23423 = CARTESIAN_POINT ( 'NONE',  ( 1.999999999999998224, -26.14374999877096784, 12.46410161513774639 ) ) ;
#23424 = VECTOR ( 'NONE', #3160, 1000.000000000000000 ) ;
#23425 = CARTESIAN_POINT ( 'NONE',  ( -1.878215178124998497, -12.25316411605951927, 4.603124999385483918 ) ) ;
#23426 = DIRECTION ( 'NONE',  ( 0.000000000000000000, 1.000000000000000000, -0.000000000000000000 ) ) ;
#23427 = CARTESIAN_POINT ( 'NONE',  ( -1.999999999999998224, -12.46410161513774639, 4.743749998770967480 ) ) ;
#23428 = ORIENTED_EDGE ( 'NONE', *, *, #10821, .T. ) ;
#23429 = DIRECTION ( 'NONE',  ( 0.000000000000000000, -0.000000000000000000, -1.000000000000000000 ) ) ;
#23430 = VECTOR ( 'NONE', #14978, 1000.000000000000000 ) ;
#23431 = ORIENTED_EDGE ( 'NONE', *, *, #23598, .F. ) ;
#23432 = CIRCLE ( 'NONE', #22595, 31.10000000000000142 ) ;
#23433 = EDGE_LOOP ( 'NONE', ( #12300, #13812, #1792, #6037 ) ) ;
#23434 = DIRECTION ( 'NONE',  ( 1.000000000000000000, 0.000000000000000000, 0.000000000000000000 ) ) ;
#23435 = ORIENTED_EDGE ( 'NONE', *, *, #21165, .F. ) ;
#23436 = CARTESIAN_POINT ( 'NONE',  ( 3.756430356249997882, -27.76562499938549067, 11.16877607737301226 ) ) ;
#23437 = ORIENTED_EDGE ( 'NONE', *, *, #10643, .T. ) ;
#23438 =( BOUNDED_SURFACE ( )  B_SPLINE_SURFACE ( 1, 2, ( 
 ( #7815, #13702, #19721, #3900, #1550, #15796, #19838, #25860, #11871, #7564, #9901, #1430, #17887, #17763, #7948, #7427, #15935, #23907, #21678, #15415, #9518, #5987, #23388, #13466, #13972, #23521, #21433, #3514, #5472, #21941, #4020, #3763, #5605, #9401, #23644, #13584, #21552, #19578, #11986, #25611, #7695, #1819, #15676, #9783, #5721, #14482, #16065, #24535, #18160, #24290, #238, #10405, #6497, #8086, #363, #16321, #6239, #2203, #10546, #2582, #12510, #24149, #16576, #8594, #24029, #8209, #6111, #14094, #2323, #4673, #8333, #12124, #20227, #16183, #10281, #22449, #6375, #19960, #20100, #10163, #18545, #14365, #14229, #22325, #12259, #4406, #12382, #18275, #627, #2064, #22059, #22200, #4287, #20347, #20485, #6620, #14609, #116, #2444, #22590, #24420, #4529, #18404, #4146, #10032, #18030, #502, #8472, #16458, #10668, #11065, #24932, #22976, #25062, #12780, #19043, #5192, #11182, #1126, #10798, #13170 ),
 ( #2707, #21139, #3212, #7011, #18659, #4805, #19166, #8715, #24673, #9101, #8860, #6761, #14747, #16702, #1259, #25204, #14997, #20751, #12652, #8988, #18790, #16847, #877, #17090, #9243, #17232, #13042, #15259, #21021, #7282, #7151, #22725, #23226, #24810, #16965, #6889, #3098, #15141, #746, #18927, #5063, #14872, #2830, #20624, #22847, #4920, #12905, #20881, #2969, #10936, #1011, #23110, #17354, #13554, #15899, #11572, #23350, #5575, #19427, #21521, #17733, #1645, #5310, #5439, #21402, #21783, #9621, #3481, #19542, #23489, #1518, #9487, #7663, #25319, #7912, #25704, #11454, #21264, #19301, #17856, #9872, #17600, #5819, #7398, #11839, #25828, #3866, #13803, #15646, #21642, #17468, #25440, #7525, #13288, #15521, #3602, #3725, #15378, #25578, #19810, #3345, #9373, #23612, #1912, #5692, #1400, #13671, #11707, #19685, #13430, #11321, #1786, #9753, #7784, #15765, #23731, #22166, #11958, #9999, #3991, #18870 ) ),
 .UNSPECIFIED., .F., .F., .F. ) 
 B_SPLINE_SURFACE_WITH_KNOTS ( ( 2, 2 ),
 ( 3, 2, 2, 2, 2, 2, 2, 2, 2, 2, 2, 2, 2, 2, 2, 2, 2, 2, 2, 2, 2, 2, 2, 2, 2, 2, 2, 2, 2, 2, 2, 2, 2, 2, 2, 2, 2, 2, 2, 2, 2, 2, 2, 2, 2, 2, 2, 2, 2, 2, 2, 2, 2, 2, 2, 2, 2, 2, 2, 2, 3 ),
 ( 0.000000000000000000, 1.000000000000000000 ),
 ( 0.000000000000000000, 0.01666666666666666644, 0.03333333333333333287, 0.05000000000000000278, 0.06666666666666666574, 0.08333333333333332871, 0.1000000000000000056, 0.1166666666666666685, 0.1333333333333333315, 0.1499999999999999944, 0.1666666666666666574, 0.1833333333333333204, 0.2000000000000000111, 0.2166666666666666741, 0.2333333333333333370, 0.2500000000000000000, 0.2666666666666666630, 0.2833333333333333259, 0.2999999999999999889, 0.3166666666666666519, 0.3333333333333333148, 0.3499999999999999778, 0.3666666666666666408, 0.3833333333333333592, 0.4000000000000000222, 0.4166666666666666852, 0.4333333333333333481, 0.4500000000000000111, 0.4666666666666666741, 0.4833333333333333370, 0.5000000000000000000, 0.5166666666666667185, 0.5333333333333333259, 0.5500000000000000444, 0.5666666666666666519, 0.5833333333333333703, 0.5999999999999999778, 0.6166666666666666963, 0.6333333333333333037, 0.6500000000000000222, 0.6666666666666666297, 0.6833333333333333481, 0.6999999999999999556, 0.7166666666666666741, 0.7333333333333332815, 0.7500000000000000000, 0.7666666666666667185, 0.7833333333333333259, 0.8000000000000000444, 0.8166666666666666519, 0.8333333333333333703, 0.8499999999999999778, 0.8666666666666666963, 0.8833333333333333037, 0.9000000000000000222, 0.9166666666666666297, 0.9333333333333333481, 0.9499999999999999556, 0.9666666666666666741, 0.9833333333333332815, 1.000000000000000000 ),
 .UNSPECIFIED. ) 
 GEOMETRIC_REPRESENTATION_ITEM ( )  RATIONAL_B_SPLINE_SURFACE ( (
 ( 1.000000000000000000, 0.8660254037844387076, 1.000000000000000000, 0.8660254037844387076, 1.000000000000000000, 0.8660254037844387076, 1.000000000000000000, 0.8660254037844387076, 1.000000000000000000, 0.8660254037844387076, 1.000000000000000000, 0.8660254037844387076, 1.000000000000000000, 0.8660254037844387076, 1.000000000000000000, 0.8660254037844387076, 1.000000000000000000, 0.8660254037844387076, 1.000000000000000000, 0.8660254037844387076, 1.000000000000000000, 0.8660254037844387076, 1.000000000000000000, 0.8660254037844387076, 1.000000000000000000, 0.8660254037844387076, 1.000000000000000000, 0.8660254037844387076, 1.000000000000000000, 0.8660254037844387076, 1.000000000000000000, 0.8660254037844387076, 1.000000000000000000, 0.8660254037844387076, 1.000000000000000000, 0.8660254037844387076, 1.000000000000000000, 0.8660254037844387076, 1.000000000000000000, 0.8660254037844387076, 1.000000000000000000, 0.8660254037844387076, 1.000000000000000000, 0.8660254037844387076, 1.000000000000000000, 0.8660254037844387076, 1.000000000000000000, 0.8660254037844387076, 1.000000000000000000, 0.8660254037844387076, 1.000000000000000000, 0.8660254037844387076, 1.000000000000000000, 0.8660254037844387076, 1.000000000000000000, 0.8660254037844387076, 1.000000000000000000, 0.8660254037844387076, 1.000000000000000000, 0.8660254037844387076, 1.000000000000000000, 0.8660254037844387076, 1.000000000000000000, 0.8660254037844387076, 1.000000000000000000, 0.8660254037844387076, 1.000000000000000000, 0.8660254037844387076, 1.000000000000000000, 0.8660254037844387076, 1.000000000000000000, 0.8660254037844387076, 1.000000000000000000, 0.8660254037844387076, 1.000000000000000000, 0.8660254037844387076, 1.000000000000000000, 0.8660254037844387076, 1.000000000000000000, 0.8660254037844387076, 1.000000000000000000, 0.8660254037844387076, 1.000000000000000000, 0.8660254037844387076, 1.000000000000000000, 0.8660254037844387076, 1.000000000000000000, 0.8660254037844387076, 1.000000000000000000, 0.8660254037844387076, 1.000000000000000000, 0.8660254037844387076, 1.000000000000000000, 0.8660254037844387076, 1.000000000000000000, 0.8660254037844387076, 1.000000000000000000, 0.8660254037844387076, 1.000000000000000000, 0.8660254037844387076, 1.000000000000000000, 0.8660254037844387076, 1.000000000000000000, 0.8660254037844387076, 1.000000000000000000, 0.8660254037844387076, 1.000000000000000000, 0.8660254037844387076, 1.000000000000000000, 0.8660254037844387076, 1.000000000000000000, 0.8660254037844387076, 1.000000000000000000, 0.8660254037844387076, 1.000000000000000000, 0.8660254037844387076, 1.000000000000000000, 0.8660254037844387076, 1.000000000000000000, 0.8660254037844387076, 1.000000000000000000),
 ( 1.000000000000000000, 0.8660254037844387076, 1.000000000000000000, 0.8660254037844387076, 1.000000000000000000, 0.8660254037844387076, 1.000000000000000000, 0.8660254037844387076, 1.000000000000000000, 0.8660254037844387076, 1.000000000000000000, 0.8660254037844387076, 1.000000000000000000, 0.8660254037844387076, 1.000000000000000000, 0.8660254037844387076, 1.000000000000000000, 0.8660254037844387076, 1.000000000000000000, 0.8660254037844387076, 1.000000000000000000, 0.8660254037844387076, 1.000000000000000000, 0.8660254037844387076, 1.000000000000000000, 0.8660254037844387076, 1.000000000000000000, 0.8660254037844387076, 1.000000000000000000, 0.8660254037844387076, 1.000000000000000000, 0.8660254037844387076, 1.000000000000000000, 0.8660254037844387076, 1.000000000000000000, 0.8660254037844387076, 1.000000000000000000, 0.8660254037844387076, 1.000000000000000000, 0.8660254037844387076, 1.000000000000000000, 0.8660254037844387076, 1.000000000000000000, 0.8660254037844387076, 1.000000000000000000, 0.8660254037844387076, 1.000000000000000000, 0.8660254037844387076, 1.000000000000000000, 0.8660254037844387076, 1.000000000000000000, 0.8660254037844387076, 1.000000000000000000, 0.8660254037844387076, 1.000000000000000000, 0.8660254037844387076, 1.000000000000000000, 0.8660254037844387076, 1.000000000000000000, 0.8660254037844387076, 1.000000000000000000, 0.8660254037844387076, 1.000000000000000000, 0.8660254037844387076, 1.000000000000000000, 0.8660254037844387076, 1.000000000000000000, 0.8660254037844387076, 1.000000000000000000, 0.8660254037844387076, 1.000000000000000000, 0.8660254037844387076, 1.000000000000000000, 0.8660254037844387076, 1.000000000000000000, 0.8660254037844387076, 1.000000000000000000, 0.8660254037844387076, 1.000000000000000000, 0.8660254037844387076, 1.000000000000000000, 0.8660254037844387076, 1.000000000000000000, 0.8660254037844387076, 1.000000000000000000, 0.8660254037844387076, 1.000000000000000000, 0.8660254037844387076, 1.000000000000000000, 0.8660254037844387076, 1.000000000000000000, 0.8660254037844387076, 1.000000000000000000, 0.8660254037844387076, 1.000000000000000000, 0.8660254037844387076, 1.000000000000000000, 0.8660254037844387076, 1.000000000000000000, 0.8660254037844387076, 1.000000000000000000, 0.8660254037844387076, 1.000000000000000000, 0.8660254037844387076, 1.000000000000000000, 0.8660254037844387076, 1.000000000000000000, 0.8660254037844387076, 1.000000000000000000, 0.8660254037844387076, 1.000000000000000000, 0.8660254037844387076, 1.000000000000000000, 0.8660254037844387076, 1.000000000000000000, 0.8660254037844387076, 1.000000000000000000, 0.8660254037844387076, 1.000000000000000000, 0.8660254037844387076, 1.000000000000000000) ) ) 
 REPRESENTATION_ITEM ( '' )  SURFACE ( )  );
#23439 = VECTOR ( 'NONE', #974, 1000.000000000000000 ) ;
#23440 = EDGE_CURVE ( 'NONE', #16647, #11238, #8079, .T. ) ;
#23441 = ORIENTED_EDGE ( 'NONE', *, *, #5767, .F. ) ;
#23442 = CARTESIAN_POINT ( 'NONE',  ( -3.999999999999997335, 28.41249999999999787, 11.30940107675849404 ) ) ;
#23443 = CARTESIAN_POINT ( 'NONE',  ( 1.500000000000001776, -7.499999999999993783, 30.00000000000000355 ) ) ;
#23444 = AXIS2_PLACEMENT_3D ( 'NONE', #22335, #10416, #18415 ) ;
#23445 = EDGE_CURVE ( 'NONE', #14404, #24819, #6719, .T. ) ;
#23446 = AXIS2_PLACEMENT_3D ( 'NONE', #15030, #1425, #25343 ) ;
#23447 = CARTESIAN_POINT ( 'NONE',  ( 3.959305671612554781E-15, 25.00000000000000000, 12.99999999999999289 ) ) ;
#23448 = CARTESIAN_POINT ( 'NONE',  ( -18.68225429291740269, -24.86329371854762016, 1.000000000000000000 ) ) ;
#23449 = CARTESIAN_POINT ( 'NONE',  ( 23.08495422774248240, 17.77255947182365503, 6.831223922626973533 ) ) ;
#23450 = VECTOR ( 'NONE', #14604, 1000.000000000000000 ) ;
#23451 = CARTESIAN_POINT ( 'NONE',  ( 0.000000000000000000, 0.000000000000000000, 19.59999999999999787 ) ) ;
#23452 = CARTESIAN_POINT ( 'NONE',  ( 4.000000000000003553, 25.44999999999999929, 8.999999999999992895 ) ) ;
#23453 = CARTESIAN_POINT ( 'NONE',  ( 15.99595368409253915, 21.30834844001121553, 8.999999999999992895 ) ) ;
#23454 = LINE ( 'NONE', #17828, #19159 ) ;
#23455 = AXIS2_PLACEMENT_3D ( 'NONE', #22403, #18008, #8422 ) ;
#23456 = ORIENTED_EDGE ( 'NONE', *, *, #23130, .T. ) ;
#23457 = ORIENTED_EDGE ( 'NONE', *, *, #19124, .T. ) ;
#23458 = CARTESIAN_POINT ( 'NONE',  ( 4.000000000000000888, 27.15624999877097423, 11.30940107675849760 ) ) ;
#23459 = AXIS2_PLACEMENT_3D ( 'NONE', #25374, #23552, #11636 ) ;
#23460 = CARTESIAN_POINT ( 'NONE',  ( -1.878215178125000939, -29.56562499938548427, 12.25316411605952283 ) ) ;
#23461 = VECTOR ( 'NONE', #24747, 1000.000000000000000 ) ;
#23462 = ORIENTED_EDGE ( 'NONE', *, *, #10386, .F. ) ;
#23463 = CARTESIAN_POINT ( 'NONE',  ( 4.000000000000003553, 26.38750000000000284, 6.690598923241489970 ) ) ;
#23464 = CARTESIAN_POINT ( 'NONE',  ( -3.756430356249996994, 28.62812499938548427, 8.999999999999992895 ) ) ;
#23465 = CARTESIAN_POINT ( 'NONE',  ( -3.834746474454188013E-15, -26.40624999877096357, 4.999999999999992006 ) ) ;
#23466 = ORIENTED_EDGE ( 'NONE', *, *, #1688, .T. ) ;
#23467 = VERTEX_POINT ( 'NONE', #15546 ) ;
#23468 = AXIS2_PLACEMENT_3D ( 'NONE', #3133, #11100, #1158 ) ;
#23469 = CARTESIAN_POINT ( 'NONE',  ( -3.999999999999996447, -8.999999999999992895, 4.668749998770968190 ) ) ;
#23470 = VERTEX_POINT ( 'NONE', #5601 ) ;
#23471 = CARTESIAN_POINT ( 'NONE',  ( 0.3342655765624356068, 38.86701176172695682, 14.62318542138302213 ) ) ;
#23472 = EDGE_CURVE ( 'NONE', #7696, #1446, #15283, .T. ) ;
#23473 = CARTESIAN_POINT ( 'NONE',  ( -1.878215178124998497, 25.89062499938548356, 12.25316411605951927 ) ) ;
#23474 = CARTESIAN_POINT ( 'NONE',  ( -1.878215178124996498, 28.44062499938548783, 5.746835883940462963 ) ) ;
#23475 = CIRCLE ( 'NONE', #8867, 0.4999999999999991673 ) ;
#23476 = CARTESIAN_POINT ( 'NONE',  ( -2.000000000000000888, -26.21874999877096712, 12.46410161513774817 ) ) ;
#23477 = CARTESIAN_POINT ( 'NONE',  ( -3.999999999999996447, 26.16250000000000497, 11.30940107675849404 ) ) ;
#23478 = VECTOR ( 'NONE', #2317, 1000.000000000000000 ) ;
#23479 = EDGE_CURVE ( 'NONE', #5355, #15216, #13319, .T. ) ;
#23480 = AXIS2_PLACEMENT_3D ( 'NONE', #13618, #14004, #10067 ) ;
#23481 = CARTESIAN_POINT ( 'NONE',  ( -1.878215178124998497, 29.04062499938548569, 12.25316411605951927 ) ) ;
#23482 = DIRECTION ( 'NONE',  ( -0.7071067811865487940, -0.7071067811865463515, 0.000000000000000000 ) ) ;
#23483 = VECTOR ( 'NONE', #6762, 1000.000000000000000 ) ;
#23484 = EDGE_CURVE ( 'NONE', #8412, #4038, #17571, .T. ) ;
#23485 = FACE_OUTER_BOUND ( 'NONE', #9710, .T. ) ;
#23486 = CARTESIAN_POINT ( 'NONE',  ( 2.672651547586948120E-15, 26.82812499938548356, 13.33755215474603162 ) ) ;
#23487 = DIRECTION ( 'NONE',  ( 0.000000000000000000, 0.000000000000000000, 1.000000000000000000 ) ) ;
#23488 = CARTESIAN_POINT ( 'NONE',  ( 20.94803839265150458, 18.11961126790524901, 12.46410161513774817 ) ) ;
#23489 = CARTESIAN_POINT ( 'NONE',  ( 19.68629472953723436, 19.68629472953716686, 13.33755215474602984 ) ) ;
#23490 = DIRECTION ( 'NONE',  ( -0.1253332335642912687, 0.9921147013144795412, 0.000000000000000000 ) ) ;
#23491 = CARTESIAN_POINT ( 'NONE',  ( -1.878215178124995832, 29.34062499938548285, 5.746835883940462963 ) ) ;
#23492 = FACE_OUTER_BOUND ( 'NONE', #10298, .T. ) ;
#23493 = CARTESIAN_POINT ( 'NONE',  ( 20.78451994863305430, 15.12766569914060888, 8.999999999999992895 ) ) ;
#23494 = EDGE_LOOP ( 'NONE', ( #13341, #6736, #450, #22887 ) ) ;
#23495 = CARTESIAN_POINT ( 'NONE',  ( -1.999999999999998224, 25.69374999877097210, 12.46410161513774639 ) ) ;
#23496 = CARTESIAN_POINT ( 'NONE',  ( -4.000000000000003553, -26.80000000000000071, 8.999999999999992895 ) ) ;
#23498 = ORIENTED_EDGE ( 'NONE', *, *, #20736, .F. ) ;
#23497 = LINE ( 'NONE', #23742, #1284 ) ;
#23499 = CARTESIAN_POINT ( 'NONE',  ( -3.756430356249996994, 25.92812499938548498, 8.999999999999992895 ) ) ;
#23500 = VECTOR ( 'NONE', #15982, 1000.000000000000000 ) ;
#23501 = DIRECTION ( 'NONE',  ( 0.000000000000000000, 0.000000000000000000, 1.000000000000000000 ) ) ;
#23502 = CARTESIAN_POINT ( 'NONE',  ( -25.83240171513484640, 3.403349963601426165, 20.00001199999999812 ) ) ;
#23503 = CARTESIAN_POINT ( 'NONE',  ( 1.071796769724494558, 26.38615380933864074, 4.999999999999992895 ) ) ;
#23504 = ORIENTED_EDGE ( 'NONE', *, *, #25617, .T. ) ;
#23505 = VERTEX_POINT ( 'NONE', #5850 ) ;
#23506 = CARTESIAN_POINT ( 'NONE',  ( -17.08421000182742233, 25.98730014090460472, -6.500000000000000000 ) ) ;
#23507 = CARTESIAN_POINT ( 'NONE',  ( 3.756430356250000546, 25.55312499938548498, 11.16877607737301226 ) ) ;
#23508 = AXIS2_PLACEMENT_3D ( 'NONE', #8429, #6461, #4367 ) ;
#23509 = DIRECTION ( 'NONE',  ( -0.000000000000000000, 0.000000000000000000, 1.000000000000000000 ) ) ;
#23510 = CIRCLE ( 'NONE', #17682, 0.4999999999999993339 ) ;
#23511 = ADVANCED_FACE ( 'NONE', ( #13967 ), #6105, .T. ) ;
#23512 = CARTESIAN_POINT ( 'NONE',  ( 3.735045420075836212E-15, -4.662447845253954171, 4.415624999385481253 ) ) ;
#23513 = SHAPE_REPRESENTATION_RELATIONSHIP ( 'NONE' , 'NONE' ,  #23199, #16592 ) ;
#23514 = CARTESIAN_POINT ( 'NONE',  ( 1.999999999999998224, -27.49374999877096926, 12.46410161513774639 ) ) ;
#23515 = EDGE_CURVE ( 'NONE', #18045, #17369, #20079, .T. ) ;
#23516 = DIRECTION ( 'NONE',  ( 0.000000000000000000, 0.000000000000000000, -1.000000000000000000 ) ) ;
#23517 = DIRECTION ( 'NONE',  ( -0.000000000000000000, -1.000000000000000000, 0.000000000000000000 ) ) ;
#23518 = CARTESIAN_POINT ( 'NONE',  ( 3.918623196469464443, 38.49999999999999289, 4.456389954662531849 ) ) ;
#23519 = CARTESIAN_POINT ( 'NONE',  ( -1.952785157361865753, -31.03863125411923463, 1.000000000000000000 ) ) ;
#23520 = CARTESIAN_POINT ( 'NONE',  ( -26.75313774936397948, 14.98253926456367502, -6.500000000000000000 ) ) ;
#23521 = CARTESIAN_POINT ( 'NONE',  ( 21.44743255599544440, 15.79057830650299721, 6.690598923241489970 ) ) ;
#23522 = ORIENTED_EDGE ( 'NONE', *, *, #1314, .T. ) ;
#23523 = CARTESIAN_POINT ( 'NONE',  ( 0.7500000000000001110, 9.184850993605150903E-17, 18.19999999999999929 ) ) ;
#23524 = DIRECTION ( 'NONE',  ( 0.000000000000000000, 0.000000000000000000, 1.000000000000000000 ) ) ;
#23525 = CARTESIAN_POINT ( 'NONE',  ( 3.756430356250004099, 27.54062499938548569, 6.831223922626973533 ) ) ;
#23526 = CARTESIAN_POINT ( 'NONE',  ( 8.831537335106614961E-15, 26.63124999877096855, 12.99999999999999112 ) ) ;
#23527 = CARTESIAN_POINT ( 'NONE',  ( 2.000000000000003997, 27.32500000000000284, 5.535898384862238508 ) ) ;
#23528 = CARTESIAN_POINT ( 'NONE',  ( 0.000000000000000000, 0.000000000000000000, 1.000000000000000000 ) ) ;
#23529 = VERTEX_POINT ( 'NONE', #8081 ) ;
#23530 = CARTESIAN_POINT ( 'NONE',  ( 1.071796769724490117, -26.87634618820330701, 4.999999999999992895 ) ) ;
#23531 = EDGE_CURVE ( 'NONE', #22278, #18677, #14235, .T. ) ;
#23532 = CARTESIAN_POINT ( 'NONE',  ( -5.201695249984999769, 38.97584342600590190, 7.139037124126438094 ) ) ;
#23534 = VERTEX_POINT ( 'NONE', #5716 ) ;
#23533 = DIRECTION ( 'NONE',  ( -0.3090169943749528914, -0.9510565162951518658, 0.000000000000000000 ) ) ;
#23535 = AXIS2_PLACEMENT_3D ( 'NONE', #20338, #4910, #24413 ) ;
#23536 = VERTEX_POINT ( 'NONE', #11865 ) ;
#23537 = ORIENTED_EDGE ( 'NONE', *, *, #1844, .F. ) ;
#23538 = EDGE_LOOP ( 'NONE', ( #8802, #17281, #8156, #12058 ) ) ;
#23539 = ORIENTED_EDGE ( 'NONE', *, *, #7122, .F. ) ;
#23540 = CARTESIAN_POINT ( 'NONE',  ( 5.577813053751546416E-15, 25.33750000000000924, 12.99999999999999289 ) ) ;
#23541 = CARTESIAN_POINT ( 'NONE',  ( -1.071796769724494558, -28.18615380933863435, 4.999999999999992895 ) ) ;
#23542 = CARTESIAN_POINT ( 'NONE',  ( 30.63887302793245482, 5.335677986744801871, 1.000000000000000000 ) ) ;
#23543 = EDGE_CURVE ( 'NONE', #3732, #12422, #19833, .T. ) ;
#23544 = CARTESIAN_POINT ( 'NONE',  ( -3.756430356249996549, 25.36562499938548854, 8.999999999999992895 ) ) ;
#23545 = CARTESIAN_POINT ( 'NONE',  ( 3.756430356250003655, -8.999999999999992895, 3.740624999385481875 ) ) ;
#23546 = CARTESIAN_POINT ( 'NONE',  ( 4.000000000000003553, -8.999999999999992895, 0.8437499987709664584 ) ) ;
#23547 = CARTESIAN_POINT ( 'NONE',  ( -30.78811501957138930, 4.393401135981437555, -2.750000000000000000 ) ) ;
#23548 = CIRCLE ( 'NONE', #6040, 31.10000000000000142 ) ;
#23549 = CARTESIAN_POINT ( 'NONE',  ( 3.756430356250002323, 28.36562499938548854, 11.16877607737301226 ) ) ;
#23550 = CIRCLE ( 'NONE', #12274, 31.10000000000000142 ) ;
#23551 = CARTESIAN_POINT ( 'NONE',  ( -3.110308778861273105, 34.50000000000000000, 14.13088484572967118 ) ) ;
#23552 = DIRECTION ( 'NONE',  ( 0.000000000000000000, 1.000000000000000000, 0.000000000000000000 ) ) ;
#23553 = CARTESIAN_POINT ( 'NONE',  ( 4.000000000000003553, -6.690598923241489970, 2.737499999999999378 ) ) ;
#23554 = CARTESIAN_POINT ( 'NONE',  ( 5.335677986744568280, -30.63887302793249745, -6.500000000000000000 ) ) ;
#23555 = CYLINDRICAL_SURFACE ( 'NONE', #22056, 31.10000000000000142 ) ;
#23556 = CARTESIAN_POINT ( 'NONE',  ( 0.000000000000000000, 0.000000000000000000, -6.500000000000000000 ) ) ;
#23557 = EDGE_CURVE ( 'NONE', #583, #1666, #8818, .T. ) ;
#23558 = CARTESIAN_POINT ( 'NONE',  ( -2.620986760973688460E-15, -26.63124999877097565, 13.61880215351699874 ) ) ;
#23559 = CARTESIAN_POINT ( 'NONE',  ( -3.756430356249995661, 27.69062499938548427, 6.831223922626973533 ) ) ;
#23560 = DIRECTION ( 'NONE',  ( 0.000000000000000000, 0.000000000000000000, 1.000000000000000000 ) ) ;
#23561 = DIRECTION ( 'NONE',  ( -0.000000000000000000, 0.000000000000000000, -1.000000000000000000 ) ) ;
#23562 = CARTESIAN_POINT ( 'NONE',  ( 3.469446951953614189E-15, 40.00000000000000000, 8.999999999999992895 ) ) ;
#23563 = ORIENTED_EDGE ( 'NONE', *, *, #5551, .T. ) ;
#23564 = EDGE_CURVE ( 'NONE', #13049, #10227, #10734, .T. ) ;
#23565 = DIRECTION ( 'NONE',  ( 0.8443279255020154084, -0.5358267949789962126, 0.000000000000000000 ) ) ;
#23566 = ORIENTED_EDGE ( 'NONE', *, *, #19677, .T. ) ;
#23567 = EDGE_CURVE ( 'NONE', #10619, #7410, #12985, .T. ) ;
#23568 = VERTEX_POINT ( 'NONE', #12254 ) ;
#23569 = DIRECTION ( 'NONE',  ( 1.000000000000000000, 0.000000000000000000, 0.000000000000000000 ) ) ;
#23570 =( GEOMETRIC_REPRESENTATION_CONTEXT ( 3 ) GLOBAL_UNCERTAINTY_ASSIGNED_CONTEXT ( ( #18824 ) ) GLOBAL_UNIT_ASSIGNED_CONTEXT ( ( #9270, #1812, #21543 ) ) REPRESENTATION_CONTEXT ( 'NONE', 'WORKASPACE' ) );
#23571 = EDGE_LOOP ( 'NONE', ( #17816, #25417, #9052, #6567 ) ) ;
#23572 = CARTESIAN_POINT ( 'NONE',  ( 3.756430356249995661, -28.14062499938548356, 6.831223922626973533 ) ) ;
#23573 = VERTEX_POINT ( 'NONE', #2318 ) ;
#23574 = CARTESIAN_POINT ( 'NONE',  ( 3.469446951953614189E-15, -8.999999999999992895, 25.00000000000000000 ) ) ;
#23575 = ORIENTED_EDGE ( 'NONE', *, *, #14777, .T. ) ;
#23576 = CARTESIAN_POINT ( 'NONE',  ( 3.752267015613588906E-15, 26.46250000000000213, 4.381197846482986158 ) ) ;
#23577 = CARTESIAN_POINT ( 'NONE',  ( -24.86329371854788661, -18.68225429291705098, -2.750000000000000000 ) ) ;
#23578 = FACE_OUTER_BOUND ( 'NONE', #17517, .T. ) ;
#23579 = CARTESIAN_POINT ( 'NONE',  ( 20.45982030258741702, 15.14742554666860208, 6.831223922626973533 ) ) ;
#23580 = FACE_OUTER_BOUND ( 'NONE', #22502, .T. ) ;
#23581 = AXIS2_PLACEMENT_3D ( 'NONE', #8465, #14989, #5054 ) ;
#23582 = CARTESIAN_POINT ( 'NONE',  ( -3.999999999999997335, 27.96250000000000213, 11.30940107675849404 ) ) ;
#23583 = CARTESIAN_POINT ( 'NONE',  ( -3.756430356249996105, -6.831223922626973533, 0.4406249993854816638 ) ) ;
#23584 = CARTESIAN_POINT ( 'NONE',  ( 23.05843772344798381, 17.74604296752915999, 8.999999999999992895 ) ) ;
#23585 = DIRECTION ( 'NONE',  ( 0.000000000000000000, -1.000000000000000000, 0.000000000000000000 ) ) ;
#23586 = ORIENTED_EDGE ( 'NONE', *, *, #20696, .T. ) ;
#23587 = EDGE_CURVE ( 'NONE', #24730, #24433, #19649, .T. ) ;
#23588 = ORIENTED_EDGE ( 'NONE', *, *, #20808, .T. ) ;
#23589 = CARTESIAN_POINT ( 'NONE',  ( -4.000000000000001776, 29.21874999877097068, 8.999999999999992895 ) ) ;
#23590 =( BOUNDED_CURVE ( )  B_SPLINE_CURVE ( 2, ( #21507, #5801, #11557, #1625, #9357 ),
 .UNSPECIFIED., .F., .F. ) 
 B_SPLINE_CURVE_WITH_KNOTS ( ( 3, 2, 3 ),
 ( 0.000000000000000000, 0.01666666666666666644, 0.02500000000000000486 ),
 .UNSPECIFIED. ) 
 CURVE ( )  GEOMETRIC_REPRESENTATION_ITEM ( )  RATIONAL_B_SPLINE_CURVE ( ( 1.000000000000000000, 0.8660254037844387076, 1.000000000000000000, 0.9330127018922194093, 0.9330127018922194093 ) ) 
 REPRESENTATION_ITEM ( '' )  );
#23591 = EDGE_CURVE ( 'NONE', #5929, #6393, #8326, .T. ) ;
#23592 = ORIENTED_EDGE ( 'NONE', *, *, #12007, .T. ) ;
#23593 = CYLINDRICAL_SURFACE ( 'NONE', #17112, 31.10000000000000142 ) ;
#23594 = CARTESIAN_POINT ( 'NONE',  ( -3.756430356249997882, 26.86562499938548498, 11.16877607737301226 ) ) ;
#23595 = CARTESIAN_POINT ( 'NONE',  ( 9.610428525060671134, -29.57785765677934009, 1.000000000000000000 ) ) ;
#23596 = ORIENTED_EDGE ( 'NONE', *, *, #4612, .T. ) ;
#23597 = ORIENTED_EDGE ( 'NONE', *, *, #7734, .T. ) ;
#23598 = EDGE_CURVE ( 'NONE', #5872, #14663, #16781, .T. ) ;
#23599 = CARTESIAN_POINT ( 'NONE',  ( 2.000000000000003997, -5.535898384862238508, 4.125000000000000000 ) ) ;
#23600 = VERTEX_POINT ( 'NONE', #8204 ) ;
#23601 = CARTESIAN_POINT ( 'NONE',  ( 3.469446951953614189E-15, 30.00000000000000355, 4.999999999999992006 ) ) ;
#23602 = CARTESIAN_POINT ( 'NONE',  ( 3.756430356250003655, 25.14062499938548356, 8.999999999999992895 ) ) ;
#23603 = CARTESIAN_POINT ( 'NONE',  ( -3.756430356249996549, 27.61562499938548143, 8.999999999999992895 ) ) ;
#23604 = CARTESIAN_POINT ( 'NONE',  ( 0.4995657836784154204, 38.49999999999999289, 3.020833333333325044 ) ) ;
#23605 = CARTESIAN_POINT ( 'NONE',  ( 4.000000000000005329, 27.73750000000000782, 6.690598923241489970 ) ) ;
#23606 = CARTESIAN_POINT ( 'NONE',  ( 3.756430356250004099, 26.07812499938548356, 6.831223922626973533 ) ) ;
#23607 =( NAMED_UNIT ( * ) SI_UNIT ( $, .STERADIAN. ) SOLID_ANGLE_UNIT ( ) );
#23608 = CARTESIAN_POINT ( 'NONE',  ( -0.4995657836784057060, 31.50000000000000000, 3.020833333333325044 ) ) ;
#23609 = AXIS2_PLACEMENT_3D ( 'NONE', #20138, #6803, #14785 ) ;
#23610 = CARTESIAN_POINT ( 'NONE',  ( -3.999999999999998224, 26.96874999877097068, 8.999999999999992895 ) ) ;
#23611 = CARTESIAN_POINT ( 'NONE',  ( 21.46069080901174786, 15.80383655951930066, 8.999999999999992895 ) ) ;
#23612 = CARTESIAN_POINT ( 'NONE',  ( 17.90514199329621903, 23.21753674921489008, 8.999999999999992895 ) ) ;
#23613 = EDGE_CURVE ( 'NONE', #13776, #15232, #23901, .T. ) ;
#23614 = CARTESIAN_POINT ( 'NONE',  ( -1.071796769724494558, -28.63615380933863364, 4.999999999999992895 ) ) ;
#23615 = CARTESIAN_POINT ( 'NONE',  ( 2.000000000000000888, 29.36874999877096926, 12.46410161513774817 ) ) ;
#23617 = ADVANCED_FACE ( 'NONE', ( #111 ), #24025, .F. ) ;
#23616 = FACE_OUTER_BOUND ( 'NONE', #10387, .T. ) ;
#23618 = DIRECTION ( 'NONE',  ( 0.000000000000000000, 0.000000000000000000, 1.000000000000000000 ) ) ;
#23619 = CARTESIAN_POINT ( 'NONE',  ( 1.071796769724492782, 25.75134618820331056, 12.99999999999999467 ) ) ;
#23620 = VERTEX_POINT ( 'NONE', #16177 ) ;
#23621 = CARTESIAN_POINT ( 'NONE',  ( 2.000000000000000888, 26.66874999877096641, 12.46410161513774817 ) ) ;
#23622 = CARTESIAN_POINT ( 'NONE',  ( -2.000000000000003997, -26.42500000000000071, 5.535898384862238508 ) ) ;
#23624 = VERTEX_POINT ( 'NONE', #21673 ) ;
#23623 = CARTESIAN_POINT ( 'NONE',  ( -1.878215178124998275, 25.55312499938549564, 12.25316411605951927 ) ) ;
#23625 = CARTESIAN_POINT ( 'NONE',  ( 1.878215178125000939, 27.87812499938548427, 12.25316411605952283 ) ) ;
#23626 = FACE_BOUND ( 'NONE', #16145, .T. ) ;
#23627 = ORIENTED_EDGE ( 'NONE', *, *, #13384, .T. ) ;
#23628 = CARTESIAN_POINT ( 'NONE',  ( 2.000000000000003553, -8.999999999999992895, 8.000000000000000000 ) ) ;
#23629 = CIRCLE ( 'NONE', #8173, 0.4999999999999999445 ) ;
#23630 = VERTEX_POINT ( 'NONE', #14224 ) ;
#23631 = ORIENTED_EDGE ( 'NONE', *, *, #9563, .F. ) ;
#23632 = CARTESIAN_POINT ( 'NONE',  ( 3.401318489841097747, 30.91344420362547396, -2.750000000000000000 ) ) ;
#23633 = CARTESIAN_POINT ( 'NONE',  ( -1.878215178124996498, 26.19062499938548783, 5.746835883940462963 ) ) ;
#23634 = ADVANCED_FACE ( 'NONE', ( #22196 ), #3758, .T. ) ;
#23635 = CARTESIAN_POINT ( 'NONE',  ( 1.878215178125000939, -12.25316411605952283, 2.765624999385481786 ) ) ;
#23636 = CARTESIAN_POINT ( 'NONE',  ( -1.999999999999998224, 28.39374999877097139, 12.46410161513774639 ) ) ;
#23637 = APPLICATION_PROTOCOL_DEFINITION ( 'draft international standard', 'automotive_design', 1998, #19446 ) ;
#23638 = CARTESIAN_POINT ( 'NONE',  ( -3.834746474454188013E-15, -27.36250000000000426, 4.999999999999992006 ) ) ;
#23639 = CARTESIAN_POINT ( 'NONE',  ( 19.29959570814131808, 22.12802283288743155, 12.46410161513774639 ) ) ;
#23640 = CARTESIAN_POINT ( 'NONE',  ( 5.532151103383248447, 31.50000000000000000, 11.32277940608563149 ) ) ;
#23641 = DIRECTION ( 'NONE',  ( 1.000000000000000000, 0.000000000000000000, 0.000000000000000000 ) ) ;
#23642 = LINE ( 'NONE', #25609, #18397 ) ;
#23643 = FACE_OUTER_BOUND ( 'NONE', #3195, .T. ) ;
#23644 = CARTESIAN_POINT ( 'NONE',  ( 20.27186753227280747, 17.44344040752655545, 12.46410161513774817 ) ) ;
#23645 = VERTEX_POINT ( 'NONE', #20876 ) ;
#23646 = DIRECTION ( 'NONE',  ( -0.000000000000000000, -0.000000000000000000, -1.000000000000000000 ) ) ;
#23647 = DIRECTION ( 'NONE',  ( -0.9822872507286872779, 0.1873813145857327056, 0.000000000000000000 ) ) ;
#23648 = CARTESIAN_POINT ( 'NONE',  ( 3.756430356250002323, 28.81562499938548427, 11.16877607737301226 ) ) ;
#23649 = CARTESIAN_POINT ( 'NONE',  ( 18.39361514561510091, 18.39361514561503341, 4.999999999999992006 ) ) ;
#23650 = DIRECTION ( 'NONE',  ( 0.000000000000000000, 0.000000000000000000, 1.000000000000000000 ) ) ;
#23651 = CARTESIAN_POINT ( 'NONE',  ( 3.110308778861349932, 38.49999999999999289, 14.13088484572963033 ) ) ;
#23652 = ORIENTED_EDGE ( 'NONE', *, *, #19386, .F. ) ;
#23653 = CARTESIAN_POINT ( 'NONE',  ( -4.000000000000043521, -11.30940107675846562, 2.512500000000000622 ) ) ;
#23654 = DIRECTION ( 'NONE',  ( -0.000000000000000000, 0.000000000000000000, -1.000000000000000000 ) ) ;
#23656 = VERTEX_POINT ( 'NONE', #4916 ) ;
#23655 = CARTESIAN_POINT ( 'NONE',  ( -2.000000000000003997, -26.42500000000000071, 5.535898384862238508 ) ) ;
#23657 = VERTEX_POINT ( 'NONE', #6370 ) ;
#23658 = ORIENTED_EDGE ( 'NONE', *, *, #2345, .F. ) ;
#23660 = EDGE_CURVE ( 'NONE', #13603, #25184, #18433, .T. ) ;
#23659 = ORIENTED_EDGE ( 'NONE', *, *, #21306, .T. ) ;
#23661 = EDGE_LOOP ( 'NONE', ( #5766, #5421, #6415, #10744 ) ) ;
#23662 = DIRECTION ( 'NONE',  ( 0.000000000000000000, 0.000000000000000000, 1.000000000000000000 ) ) ;
#23663 = CARTESIAN_POINT ( 'NONE',  ( -3.110308778861273105, 38.49999999999999289, 14.13088484572967118 ) ) ;
#23664 = CARTESIAN_POINT ( 'NONE',  ( 0.7500000000000000000, -1.299038105676658450, 18.19999999999999929 ) ) ;
#23666 = EDGE_CURVE ( 'NONE', #16184, #5209, #24286, .T. ) ;
#23665 = CARTESIAN_POINT ( 'NONE',  ( 23.26836714124207361, 18.93629030671969460, 11.57226653943513028 ) ) ;
#23667 = CARTESIAN_POINT ( 'NONE',  ( 1.878215178125004048, -5.746835883940462963, 3.365624999385481875 ) ) ;
#23668 = CARTESIAN_POINT ( 'NONE',  ( 4.000000000000001776, -11.30940107675849760, 3.506249998770968102 ) ) ;
#23669 = CARTESIAN_POINT ( 'NONE',  ( 3.735045420075836212E-15, 27.16562499938548569, 4.662447845253954171 ) ) ;
#23670 = DIRECTION ( 'NONE',  ( 0.000000000000000000, 0.000000000000000000, 1.000000000000000000 ) ) ;
#23671 = DIRECTION ( 'NONE',  ( 0.000000000000000000, -0.000000000000000000, -1.000000000000000000 ) ) ;
#23672 = CARTESIAN_POINT ( 'NONE',  ( 3.752267015613588906E-15, -4.381197846482986158, 1.462499999999998135 ) ) ;
#23673 = CARTESIAN_POINT ( 'NONE',  ( 0.000000000000000000, 0.000000000000000000, 19.50000000000000000 ) ) ;
#23674 = CARTESIAN_POINT ( 'NONE',  ( -4.000000000000021316, -11.30940107675847806, 2.456249998770964282 ) ) ;
#23675 = CARTESIAN_POINT ( 'NONE',  ( 4.000000000000002665, 27.66249999999999787, 11.30940107675849760 ) ) ;
#23676 = CARTESIAN_POINT ( 'NONE',  ( 1.999999999999998224, -25.69374999877097210, 12.46410161513774639 ) ) ;
#23677 = CARTESIAN_POINT ( 'NONE',  ( 3.756430356250003655, 28.85312499938548569, 8.999999999999992895 ) ) ;
#23678 = CARTESIAN_POINT ( 'NONE',  ( -5.840899737312955864, 38.49999999999999289, 10.37254881831481512 ) ) ;
#23679 = DIRECTION ( 'NONE',  ( 0.000000000000000000, 0.000000000000000000, -1.000000000000000000 ) ) ;
#23680 = ORIENTED_EDGE ( 'NONE', *, *, #25683, .T. ) ;
#23681 = CARTESIAN_POINT ( 'NONE',  ( 2.000000000000003997, 28.67500000000000426, 5.535898384862238508 ) ) ;
#23682 = EDGE_LOOP ( 'NONE', ( #8225, #19216 ) ) ;
#23683 = ORIENTED_EDGE ( 'NONE', *, *, #2804, .F. ) ;
#23684 = FACE_OUTER_BOUND ( 'NONE', #17514, .T. ) ;
#23685 = ORIENTED_EDGE ( 'NONE', *, *, #4088, .T. ) ;
#23686 = CARTESIAN_POINT ( 'NONE',  ( -1.878215178125000939, -26.97812499938548569, 12.25316411605952283 ) ) ;
#23687 = ORIENTED_EDGE ( 'NONE', *, *, #14503, .T. ) ;
#23688 = CARTESIAN_POINT ( 'NONE',  ( -3.834746474454188013E-15, -26.01249999999999574, 4.999999999999992006 ) ) ;
#23689 = EDGE_CURVE ( 'NONE', #22273, #5799, #24702, .T. ) ;
#23690 = ORIENTED_EDGE ( 'NONE', *, *, #10022, .T. ) ;
#23691 = ADVANCED_FACE ( 'NONE', ( #14868 ), #22843, .F. ) ;
#23692 = CARTESIAN_POINT ( 'NONE',  ( -3.999999999999996447, 27.47499999999999787, 8.999999999999992895 ) ) ;
#23693 = LINE ( 'NONE', #7867, #9735 ) ;
#23694 = CARTESIAN_POINT ( 'NONE',  ( -3.756430356249996994, -8.999999999999992895, 1.378124999385485605 ) ) ;
#23695 = FACE_OUTER_BOUND ( 'NONE', #14165, .T. ) ;
#23696 = CARTESIAN_POINT ( 'NONE',  ( 15.30652457243565223, 20.61891932835433394, 11.16877607737301226 ) ) ;
#23697 = EDGE_CURVE ( 'NONE', #25812, #25396, #12505, .T. ) ;
#23698 = CARTESIAN_POINT ( 'NONE',  ( -0.5000000000000000000, -0.8660254037844387076, 19.50000000000000000 ) ) ;
#23699 = CYLINDRICAL_SURFACE ( 'NONE', #18821, 4.000000000000000000 ) ;
#23700 = CARTESIAN_POINT ( 'NONE',  ( 2.620986760973688460E-15, 28.93750000000000000, 13.61880215351699874 ) ) ;
#23701 = CARTESIAN_POINT ( 'NONE',  ( -3.999999999999996447, 29.27500000000000213, 8.999999999999992895 ) ) ;
#23702 = CARTESIAN_POINT ( 'NONE',  ( 18.96807563933094798, 21.62427301729024975, 12.25316411605951927 ) ) ;
#23703 = CARTESIAN_POINT ( 'NONE',  ( 1.071796769724496334, 28.24240381056767291, 4.999999999999992895 ) ) ;
#23704 = EDGE_LOOP ( 'NONE', ( #8663, #5357, #21345, #6042 ) ) ;
#23705 = EDGE_LOOP ( 'NONE', ( #10847, #7931, #3884, #9028 ) ) ;
#23706 = CARTESIAN_POINT ( 'NONE',  ( 4.000000000000005329, 29.48124999877097707, 6.690598923241489970 ) ) ;
#23707 = VERTEX_POINT ( 'NONE', #20480 ) ;
#23708 = DIRECTION ( 'NONE',  ( 0.000000000000000000, 0.000000000000000000, 1.000000000000000000 ) ) ;
#23709 = CARTESIAN_POINT ( 'NONE',  ( -1.071796769724487897, 29.36740381056767291, 12.99999999999999289 ) ) ;
#23710 = DIRECTION ( 'NONE',  ( 0.000000000000000000, 0.000000000000000000, 1.000000000000000000 ) ) ;
#23711 = VERTEX_POINT ( 'NONE', #24416 ) ;
#23712 = VERTEX_POINT ( 'NONE', #14478 ) ;
#23713 = CIRCLE ( 'NONE', #9097, 0.4999999999999998890 ) ;
#23714 = DIRECTION ( 'NONE',  ( 0.000000000000000000, 0.000000000000000000, 1.000000000000000000 ) ) ;
#23715 = ORIENTED_EDGE ( 'NONE', *, *, #9365, .F. ) ;
#23716 = CARTESIAN_POINT ( 'NONE',  ( 1.453535542772610212, 31.06601413805602263, 1.000000000000000000 ) ) ;
#23717 = CARTESIAN_POINT ( 'NONE',  ( 3.756430356250002323, 25.55312499938548143, 11.16877607737301226 ) ) ;
#23718 = CARTESIAN_POINT ( 'NONE',  ( -1.878215178124999829, 29.04062499938549280, 12.25316411605951927 ) ) ;
#23719 = AXIS2_PLACEMENT_3D ( 'NONE', #273, #21975, #1719 ) ;
#23720 = DIRECTION ( 'NONE',  ( 0.000000000000000000, 0.000000000000000000, 1.000000000000000000 ) ) ;
#23721 = CARTESIAN_POINT ( 'NONE',  ( 0.000000000000000000, 26.68750000000000711, 13.61880215351699874 ) ) ;
#23722 = ADVANCED_FACE ( 'NONE', ( #2825 ), #2703, .F. ) ;
#23723 = EDGE_CURVE ( 'NONE', #9415, #10323, #483, .T. ) ;
#23724 = CARTESIAN_POINT ( 'NONE',  ( -1.878215178124998497, 25.89062499938548356, 12.25316411605951927 ) ) ;
#23725 = CARTESIAN_POINT ( 'NONE',  ( 16.23990935651717393, 26.52310962334745170, 1.000000000000000000 ) ) ;
#23726 = LINE ( 'NONE', #80, #11735 ) ;
#23727 = VECTOR ( 'NONE', #8372, 1000.000000000000000 ) ;
#23728 = AXIS2_PLACEMENT_3D ( 'NONE', #15519, #23487, #15897 ) ;
#23729 = CARTESIAN_POINT ( 'NONE',  ( 0.000000000000000000, 0.000000000000000000, 1.000000000000000000 ) ) ;
#23730 = CARTESIAN_POINT ( 'NONE',  ( 18.38477631085027753, 21.21320343559639454, 12.46410161513774639 ) ) ;
#23731 = CARTESIAN_POINT ( 'NONE',  ( 18.24985654912466515, 23.56225130504333976, 11.16877607737301226 ) ) ;
#23732 = DIRECTION ( 'NONE',  ( 0.000000000000000000, 0.000000000000000000, 1.000000000000000000 ) ) ;
#23733 = CARTESIAN_POINT ( 'NONE',  ( 3.756430356250003655, 29.19062499938548072, 8.999999999999992895 ) ) ;
#23735 = CARTESIAN_POINT ( 'NONE',  ( 2.620986760973688460E-15, -13.61880215351699874, 2.981249998770965970 ) ) ;
#23734 = VECTOR ( 'NONE', #9707, 1000.000000000000000 ) ;
#23736 = DIRECTION ( 'NONE',  ( -0.000000000000000000, 0.000000000000000000, -1.000000000000000000 ) ) ;
#23737 = FACE_OUTER_BOUND ( 'NONE', #1054, .T. ) ;
#23738 = AXIS2_PLACEMENT_3D ( 'NONE', #15288, #9517, #11356 ) ;
#23739 = ORIENTED_EDGE ( 'NONE', *, *, #23666, .T. ) ;
#23740 = CARTESIAN_POINT ( 'NONE',  ( -3.999999999999997335, 27.90624999877097068, 11.30940107675849404 ) ) ;
#23741 = CARTESIAN_POINT ( 'NONE',  ( -2.620986760973688460E-15, -26.23750000000000071, 13.61880215351699874 ) ) ;
#23743 = EDGE_LOOP ( 'NONE', ( #14831, #13119, #13054, #6032, #12179, #9381, #9560, #640, #1029, #17658, #6604, #24521, #24078, #20534, #20009, #794, #15658, #551, #7447, #7380, #15881, #22254, #21527, #213, #20825 ) ) ;
#23742 = CARTESIAN_POINT ( 'NONE',  ( -3.526711513754876570, 29.50000000000000000, 4.645898033750338385 ) ) ;
#23744 = CARTESIAN_POINT ( 'NONE',  ( -3.756430356249996105, 28.59062499938548640, 6.831223922626973533 ) ) ;
#23745 = CARTESIAN_POINT ( 'NONE',  ( 1.057460391440397258E-14, -29.55624999877096926, 4.999999999999992006 ) ) ;
#23746 = CARTESIAN_POINT ( 'NONE',  ( 1.701696020694463574, 25.99999999999999645, 20.00001200000000168 ) ) ;
#23747 = CARTESIAN_POINT ( 'NONE',  ( -3.999999999999996447, -8.999999999999992895, 1.968749998770967569 ) ) ;
#23748 = ORIENTED_EDGE ( 'NONE', *, *, #23084, .T. ) ;
#23749 = ORIENTED_EDGE ( 'NONE', *, *, #8496, .F. ) ;
#23750 = DIRECTION ( 'NONE',  ( 0.000000000000000000, -0.000000000000000000, 1.000000000000000000 ) ) ;
#23751 = CARTESIAN_POINT ( 'NONE',  ( -3.756430356249996105, 29.49062499938548854, 6.831223922626973533 ) ) ;
#23752 = VECTOR ( 'NONE', #18584, 1000.000000000000000 ) ;
#23753 = EDGE_CURVE ( 'NONE', #22016, #17650, #1317, .T. ) ;
#23754 = AXIS2_PLACEMENT_3D ( 'NONE', #23253, #1678, #7424 ) ;
#23755 = CARTESIAN_POINT ( 'NONE',  ( -1.878215178124995832, -5.746835883940462963, 3.890624999385482674 ) ) ;
#23757 = EDGE_CURVE ( 'NONE', #5938, #3647, #18655, .T. ) ;
#23756 = CIRCLE ( 'NONE', #20000, 30.10000000000000142 ) ;
#23758 = VECTOR ( 'NONE', #7701, 1000.000000000000000 ) ;
#23759 = CARTESIAN_POINT ( 'NONE',  ( 26.49999999999999645, -0.5000000000000000000, 19.50000000000000000 ) ) ;
#23760 = DIRECTION ( 'NONE',  ( -0.2486898871648449971, 0.9685831611286336296, 0.000000000000000000 ) ) ;
#23761 = DIRECTION ( 'NONE',  ( 1.000000000000000000, 0.000000000000000000, 0.000000000000000000 ) ) ;
#23762 = DIRECTION ( 'NONE',  ( -0.000000000000000000, 0.000000000000000000, 1.000000000000000000 ) ) ;
#23763 = CARTESIAN_POINT ( 'NONE',  ( 3.834746474454188013E-15, 27.36250000000000071, 4.999999999999992006 ) ) ;
#23764 = CARTESIAN_POINT ( 'NONE',  ( 2.000000000000003997, 25.52500000000000213, 5.535898384862238508 ) ) ;
#23765 = CARTESIAN_POINT ( 'NONE',  ( 2.000000000000000888, -12.46410161513774817, 2.118749998770968368 ) ) ;
#23766 = DIRECTION ( 'NONE',  ( 0.000000000000000000, 0.000000000000000000, 1.000000000000000000 ) ) ;
#23767 = ORIENTED_EDGE ( 'NONE', *, *, #9443, .T. ) ;
#23768 = DIRECTION ( 'NONE',  ( 1.000000000000000000, 0.000000000000000000, 0.000000000000000000 ) ) ;
#23769 = CARTESIAN_POINT ( 'NONE',  ( 1.626862140677534194E-14, 28.03750000000000497, 12.99999999999999289 ) ) ;
#23770 = CARTESIAN_POINT ( 'NONE',  ( -1.878215178124995832, 27.65312499938548640, 5.746835883940462963 ) ) ;
#23772 = EDGE_CURVE ( 'NONE', #4730, #13467, #10932, .T. ) ;
#23771 = DIRECTION ( 'NONE',  ( -0.000000000000000000, -0.000000000000000000, 1.000000000000000000 ) ) ;
#23773 = CARTESIAN_POINT ( 'NONE',  ( -21.65113613650350288, -22.32573188046905344, 1.000000000000000000 ) ) ;
#23774 = DIRECTION ( 'NONE',  ( -0.000000000000000000, -0.000000000000000000, 1.000000000000000000 ) ) ;
#23775 = ORIENTED_EDGE ( 'NONE', *, *, #18928, .F. ) ;
#23776 = CARTESIAN_POINT ( 'NONE',  ( 4.000000000000001776, 27.21250000000000213, 11.30940107675849760 ) ) ;
#23777 = DIRECTION ( 'NONE',  ( -1.000000000000000000, 0.000000000000000000, 0.000000000000000000 ) ) ;
#23779 = ORIENTED_EDGE ( 'NONE', *, *, #20242, .T. ) ;
#23778 = CARTESIAN_POINT ( 'NONE',  ( 1.999999999999998224, -26.59374999877096712, 12.46410161513774639 ) ) ;
#23780 = CIRCLE ( 'NONE', #7101, 0.5000000000000011102 ) ;
#23781 = VERTEX_POINT ( 'NONE', #4800 ) ;
#23783 = ORIENTED_EDGE ( 'NONE', *, *, #204, .F. ) ;
#23782 = AXIS2_PLACEMENT_3D ( 'NONE', #3995, #19933, #22700 ) ;
#23784 = EDGE_LOOP ( 'NONE', ( #10175, #6451, #11261, #13747 ) ) ;
#23785 = ORIENTED_EDGE ( 'NONE', *, *, #2510, .F. ) ;
#23786 = CARTESIAN_POINT ( 'NONE',  ( 2.451530025008918923, -31.00322564728515928, 1.000000000000000000 ) ) ;
#23787 = CARTESIAN_POINT ( 'NONE',  ( 28.72825533807133169, 11.91206721063041485, -2.750000000000000000 ) ) ;
#23788 = AXIS2_PLACEMENT_3D ( 'NONE', #11368, #11107, #15182 ) ;
#23789 = SURFACE_SIDE_STYLE ('',( #10054 ) ) ;
#23790 = CARTESIAN_POINT ( 'NONE',  ( 3.756430356250002323, 27.35312499938548569, 11.16877607737301226 ) ) ;
#23791 = MECHANICAL_DESIGN_GEOMETRIC_PRESENTATION_REPRESENTATION (  '', ( #5405 ), #25865 ) ;
#23792 = AXIS2_PLACEMENT_3D ( 'NONE', #22737, #22989, #18671 ) ;
#23793 = CARTESIAN_POINT ( 'NONE',  ( 1.878215178125000939, -12.25316411605952283, 2.765624999385481786 ) ) ;
#23794 = CARTESIAN_POINT ( 'NONE',  ( 2.000000000000000888, -12.46410161513774817, 3.918749998770967746 ) ) ;
#23795 = CARTESIAN_POINT ( 'NONE',  ( 3.756430356250004099, 28.44062499938548783, 6.831223922626973533 ) ) ;
#23796 = VECTOR ( 'NONE', #4741, 1000.000000000000000 ) ;
#23797 = EDGE_CURVE ( 'NONE', #19408, #4579, #8467, .T. ) ;
#23798 = CARTESIAN_POINT ( 'NONE',  ( -30.35476721088022600, 3.897863563850190616, -6.500000000000000000 ) ) ;
#23799 = CARTESIAN_POINT ( 'NONE',  ( -19.82388608118446527, -23.96296185032687376, -6.500000000000000000 ) ) ;
#23800 = CIRCLE ( 'NONE', #1195, 0.5000000000000001110 ) ;
#23801 = CARTESIAN_POINT ( 'NONE',  ( -3.999999999999996447, -8.999999999999992895, 1.125000000000000888 ) ) ;
#23802 = CARTESIAN_POINT ( 'NONE',  ( 31.09598070739550479, 0.4999838450258677902, -6.500000000000000000 ) ) ;
#23803 = CARTESIAN_POINT ( 'NONE',  ( 1.071796769724494336, 25.75134618820330346, 12.99999999999999467 ) ) ;
#23804 = CARTESIAN_POINT ( 'NONE',  ( 3.469446951953614189E-15, 31.50000000000000000, 8.999999999999992895 ) ) ;
#23805 = CARTESIAN_POINT ( 'NONE',  ( 3.999999999999996447, -28.31874999877096855, 8.999999999999992895 ) ) ;
#23806 = CARTESIAN_POINT ( 'NONE',  ( 1.878215178125000939, 28.77812499938548640, 12.25316411605952283 ) ) ;
#23807 = CARTESIAN_POINT ( 'NONE',  ( -3.834746474454188013E-15, -26.01249999999999574, 4.999999999999992006 ) ) ;
#23808 = AXIS2_PLACEMENT_3D ( 'NONE', #2807, #5173, #8968 ) ;
#23809 = DIRECTION ( 'NONE',  ( 0.000000000000000000, -1.000000000000000000, 0.000000000000000000 ) ) ;
#23810 = CARTESIAN_POINT ( 'NONE',  ( -1.859271017917182139E-15, -26.18124999877096570, 12.99999999999999289 ) ) ;
#23811 = ORIENTED_EDGE ( 'NONE', *, *, #11708, .F. ) ;
#23812 = CARTESIAN_POINT ( 'NONE',  ( -4.000000000000003553, -29.08750000000000213, 6.690598923241489970 ) ) ;
#23813 = EDGE_LOOP ( 'NONE', ( #15598, #15390, #4060, #17305, #8376 ) ) ;
#23814 =( BOUNDED_CURVE ( )  B_SPLINE_CURVE ( 2, ( #6373, #24288, #22057, #8207, #8084, #22323, #23764, #2062, #10279 ),
 .UNSPECIFIED., .F., .F. ) 
 B_SPLINE_CURVE_WITH_KNOTS ( ( 3, 2, 2, 2, 3 ),
 ( 0.07500000000000001110, 0.08333333333333332871, 0.1000000000000000056, 0.1166666666666666685, 0.1250000000000000000 ),
 .UNSPECIFIED. ) 
 CURVE ( )  GEOMETRIC_REPRESENTATION_ITEM ( )  RATIONAL_B_SPLINE_CURVE ( ( 0.9330127018922192983, 0.9330127018922194093, 1.000000000000000000, 0.8660254037844387076, 1.000000000000000000, 0.8660254037844387076, 1.000000000000000000, 0.9330127018922194093, 0.9330127018922194093 ) ) 
 REPRESENTATION_ITEM ( '' )  );
#23815 = AXIS2_PLACEMENT_3D ( 'NONE', #6895, #7016, #14878 ) ;
#23816 = EDGE_LOOP ( 'NONE', ( #19059, #11016, #14164 ) ) ;
#23817 = DIRECTION ( 'NONE',  ( 0.000000000000000000, 1.000000000000000000, 0.000000000000000000 ) ) ;
#23818 = EDGE_LOOP ( 'NONE', ( #10424, #5353, #12878, #17692, #10236, #20301, #9468, #2142, #15416, #10650, #8613, #16786, #13597, #8951, #24728, #2332, #20936, #12400, #2945, #3648, #15158, #20467, #7965 ) ) ;
#23819 = CARTESIAN_POINT ( 'NONE',  ( -1.878215178125004048, -27.57812499938548711, 5.746835883940462963 ) ) ;
#23820 = CLOSED_SHELL ( 'NONE', ( #6906, #10438, #3099, #11861, #16726, #102, #9722, #7974, #11691, #17046, #10316 ) ) ;
#23821 = ORIENTED_EDGE ( 'NONE', *, *, #24350, .T. ) ;
#23822 = FACE_OUTER_BOUND ( 'NONE', #25363, .T. ) ;
#23823 = AXIS2_PLACEMENT_3D ( 'NONE', #5246, #15197, #19481 ) ;
#23824 = VERTEX_POINT ( 'NONE', #18785 ) ;
#23825 = CARTESIAN_POINT ( 'NONE',  ( 2.000000000000000888, 29.81874999877096855, 12.46410161513774817 ) ) ;
#23826 = CARTESIAN_POINT ( 'NONE',  ( 1.878215178125004048, 26.67812499938548498, 5.746835883940462963 ) ) ;
#23827 = CARTESIAN_POINT ( 'NONE',  ( -1.878215178124998497, -12.25316411605951927, 1.003124999385485161 ) ) ;
#23828 = CYLINDRICAL_SURFACE ( 'NONE', #18354, 4.000000000000000000 ) ;
#23829 = CARTESIAN_POINT ( 'NONE',  ( 22.71372316761954124, 17.40132841170072808, 11.16877607737301226 ) ) ;
#23830 = CIRCLE ( 'NONE', #14659, 0.4999999999999986122 ) ;
#23831 = CYLINDRICAL_SURFACE ( 'NONE', #13809, 31.10000000000000142 ) ;
#23832 = EDGE_CURVE ( 'NONE', #4688, #22740, #8856, .T. ) ;
#23833 = CYLINDRICAL_SURFACE ( 'NONE', #9612, 0.5000000000000004441 ) ;
#23834 = CARTESIAN_POINT ( 'NONE',  ( -3.999999999999996003, 29.23750000000000071, 6.690598923241487306 ) ) ;
#23835 = AXIS2_PLACEMENT_3D ( 'NONE', #14347, #8069, #18147 ) ;
#23836 = VECTOR ( 'NONE', #4314, 1000.000000000000000 ) ;
#23837 = CARTESIAN_POINT ( 'NONE',  ( 3.756430356250003655, -8.999999999999992895, 0.7031249993854835623 ) ) ;
#23838 = ADVANCED_FACE ( 'NONE', ( #624 ), #2439, .T. ) ;
#23839 = CARTESIAN_POINT ( 'NONE',  ( 0.7500000000000000000, -2.999999999999999556, 17.69999999999999929 ) ) ;
#23840 = CARTESIAN_POINT ( 'NONE',  ( -28.91604871112448549, 11.44867358849382910, -6.500000000000000000 ) ) ;
#23841 = VERTEX_POINT ( 'NONE', #10664 ) ;
#23843 = EDGE_CURVE ( 'NONE', #21381, #24200, #24530, .T. ) ;
#23842 = ORIENTED_EDGE ( 'NONE', *, *, #6754, .F. ) ;
#23844 = CARTESIAN_POINT ( 'NONE',  ( 1.878215178125008489, 26.22812499938548925, 5.746835883940462963 ) ) ;
#23845 = CIRCLE ( 'NONE', #9664, 31.10000000000000142 ) ;
#23846 = VERTEX_POINT ( 'NONE', #12777 ) ;
#23847 = DIRECTION ( 'NONE',  ( 0.000000000000000000, 1.000000000000000000, 0.000000000000000000 ) ) ;
#23848 = CARTESIAN_POINT ( 'NONE',  ( 3.756430356250004099, 26.64062499938549067, 6.831223922626973533 ) ) ;
#23849 = CARTESIAN_POINT ( 'NONE',  ( 18.35384038830430597, 18.35384038830423492, 4.999999999999992006 ) ) ;
#23850 = DIRECTION ( 'NONE',  ( 0.000000000000000000, 0.000000000000000000, 1.000000000000000000 ) ) ;
#23851 = EDGE_CURVE ( 'NONE', #446, #2329, #16454, .T. ) ;
#23852 = ORIENTED_EDGE ( 'NONE', *, *, #4493, .F. ) ;
#23853 = ORIENTED_EDGE ( 'NONE', *, *, #649, .T. ) ;
#23854 = VECTOR ( 'NONE', #11573, 1000.000000000000000 ) ;
#23855 = AXIS2_PLACEMENT_3D ( 'NONE', #6234, #21936, #25729 ) ;
#23856 = CARTESIAN_POINT ( 'NONE',  ( 3.999999999999996447, -25.67500000000000071, 8.999999999999992895 ) ) ;
#23857 = EDGE_LOOP ( 'NONE', ( #554, #7635, #18084, #23597 ) ) ;
#23858 = CARTESIAN_POINT ( 'NONE',  ( 3.068624420619302740, 38.57523615308659970, 3.931826694835521163 ) ) ;
#23859 = DIRECTION ( 'NONE',  ( -0.000000000000000000, 0.000000000000000000, -1.000000000000000000 ) ) ;
#23860 = CARTESIAN_POINT ( 'NONE',  ( 3.756430356250004099, 28.70312499938548356, 11.16877607737301403 ) ) ;
#23861 = VECTOR ( 'NONE', #3340, 1000.000000000000000 ) ;
#23862 = CARTESIAN_POINT ( 'NONE',  ( 3.137519842735244810E-15, -26.91249999999999787, 4.999999999999991118 ) ) ;
#23863 = CYLINDRICAL_SURFACE ( 'NONE', #12499, 0.5000000000000004441 ) ;
#23864 = CARTESIAN_POINT ( 'NONE',  ( 2.000000000000000000, 28.07500000000000995, 12.46410161513774817 ) ) ;
#23865 = CIRCLE ( 'NONE', #9682, 0.4999999999999991118 ) ;
#23866 = CARTESIAN_POINT ( 'NONE',  ( -1.878215178124995832, 25.29062499938548569, 5.746835883940462963 ) ) ;
#23867 = AXIS2_PLACEMENT_3D ( 'NONE', #2214, #16192, #7959 ) ;
#23868 = CIRCLE ( 'NONE', #922, 31.10000000000000142 ) ;
#23869 = CARTESIAN_POINT ( 'NONE',  ( 3.834746474454188013E-15, 27.36250000000000426, 4.999999999999992006 ) ) ;
#23870 = CARTESIAN_POINT ( 'NONE',  ( -26.75313774936430633, -14.98253926456308172, -6.500000000000000000 ) ) ;
#23871 = CARTESIAN_POINT ( 'NONE',  ( 18.06657825931632999, 20.89500538406245056, 12.46410161513774639 ) ) ;
#23872 = AXIS2_PLACEMENT_3D ( 'NONE', #14026, #4337, #4069 ) ;
#23873 = DIRECTION ( 'NONE',  ( 1.000000000000000000, 0.000000000000000000, 0.000000000000000000 ) ) ;
#23874 = EDGE_CURVE ( 'NONE', #3881, #22864, #21516, .T. ) ;
#23875 = CARTESIAN_POINT ( 'NONE',  ( 31.09598070739550479, 0.4999838450258677902, 1.000000000000000000 ) ) ;
#23876 = CARTESIAN_POINT ( 'NONE',  ( 1.626862140677534194E-14, 28.03750000000000497, 12.99999999999999289 ) ) ;
#23877 = CARTESIAN_POINT ( 'NONE',  ( -30.53863125411922752, 1.952785157361987878, -6.500000000000000000 ) ) ;
#23878 = CARTESIAN_POINT ( 'NONE',  ( 22.02202058170775345, 19.36582320374829891, 5.746835883940462963 ) ) ;
#23879 = ORIENTED_EDGE ( 'NONE', *, *, #22102, .T. ) ;
#23880 = CARTESIAN_POINT ( 'NONE',  ( 3.752267015613588906E-15, 26.85624999877096641, 4.381197846482986158 ) ) ;
#23881 = CARTESIAN_POINT ( 'NONE',  ( -2.000000000000003997, -26.87500000000000355, 5.535898384862238508 ) ) ;
#23882 = EDGE_CURVE ( 'NONE', #20963, #8492, #25198, .T. ) ;
#23884 = VERTEX_POINT ( 'NONE', #1514 ) ;
#23883 = CARTESIAN_POINT ( 'NONE',  ( 3.469446951953614189E-15, 34.00000000000000000, 8.999999999999992895 ) ) ;
#23885 = CARTESIAN_POINT ( 'NONE',  ( 3.756430356250002323, 28.81562499938548427, 11.16877607737301403 ) ) ;
#23886 = ADVANCED_FACE ( 'NONE', ( #21259 ), #7147, .T. ) ;
#23888 = AXIS2_PLACEMENT_3D ( 'NONE', #16410, #24378, #23887 ) ;
#23887 = DIRECTION ( 'NONE',  ( 1.000000000000000000, 0.000000000000000000, -0.000000000000000000 ) ) ;
#23889 = CARTESIAN_POINT ( 'NONE',  ( 3.469446951953614189E-15, -8.999999999999992895, 6.000000000000000000 ) ) ;
#23890 = DIRECTION ( 'NONE',  ( 1.387778780781445044E-14, 1.000000000000000000, 0.000000000000000000 ) ) ;
#23891 = ORIENTED_EDGE ( 'NONE', *, *, #9608, .T. ) ;
#23892 = ORIENTED_EDGE ( 'NONE', *, *, #15880, .F. ) ;
#23893 = CARTESIAN_POINT ( 'NONE',  ( 3.469446951953614189E-15, 38.49999999999999289, 8.999999999999992895 ) ) ;
#23894 = AXIS2_PLACEMENT_3D ( 'NONE', #20910, #6523, #24704 ) ;
#23895 = CARTESIAN_POINT ( 'NONE',  ( 1.878215178125003382, 26.11562499938548854, 5.746835883940462963 ) ) ;
#23896 = CARTESIAN_POINT ( 'NONE',  ( 1.878215178125000939, -12.25316411605952283, 3.215624999385484184 ) ) ;
#23897 = AXIS2_PLACEMENT_3D ( 'NONE', #4167, #648, #16596 ) ;
#23898 = AXIS2_PLACEMENT_3D ( 'NONE', #17979, #22288, #4488 ) ;
#23899 = CYLINDRICAL_SURFACE ( 'NONE', #18779, 0.5000000000000004441 ) ;
#23900 = DIRECTION ( 'NONE',  ( -0.000000000000000000, -0.000000000000000000, -1.000000000000000000 ) ) ;
#23901 = LINE ( 'NONE', #12120, #4238 ) ;
#23902 = VECTOR ( 'NONE', #14923, 1000.000000000000000 ) ;
#23903 = CARTESIAN_POINT ( 'NONE',  ( 4.000000000000002665, 29.40624999877096357, 11.30940107675849760 ) ) ;
#23904 = DIRECTION ( 'NONE',  ( -0.000000000000000000, -0.000000000000000000, 1.000000000000000000 ) ) ;
#23905 = DIRECTION ( 'NONE',  ( 0.000000000000000000, 0.000000000000000000, 1.000000000000000000 ) ) ;
#23906 = CARTESIAN_POINT ( 'NONE',  ( 19.15823811790222919, 16.50204073994278531, 5.746835883940462963 ) ) ;
#23907 = CARTESIAN_POINT ( 'NONE',  ( 15.57844627214710975, 21.23530052163942372, 6.690598923241487306 ) ) ;
#23908 = ORIENTED_EDGE ( 'NONE', *, *, #19511, .T. ) ;
#23909 = CARTESIAN_POINT ( 'NONE',  ( -5.480138960579897578, 38.55544002051693298, 11.30344864665788585 ) ) ;
#23910 = CARTESIAN_POINT ( 'NONE',  ( 2.645323980344223447, 29.88371542788442881, 5.988343842124890237 ) ) ;
#23911 = CARTESIAN_POINT ( 'NONE',  ( 1.878215178125004048, 27.57812499938548711, 5.746835883940462963 ) ) ;
#23912 = CARTESIAN_POINT ( 'NONE',  ( 0.000000000000000000, 29.50000000000000000, 14.99999999999999289 ) ) ;
#23913 = CARTESIAN_POINT ( 'NONE',  ( -1.999999999999995781, 26.44374999877096855, 5.535898384862237620 ) ) ;
#23914 = CARTESIAN_POINT ( 'NONE',  ( 3.469446951953614189E-15, 35.50000000000000711, 4.999999999999992006 ) ) ;
#23915 = EDGE_LOOP ( 'NONE', ( #10233, #12140, #2369, #10846, #2884, #25494, #20082, #10683, #2117 ) ) ;
#23916 = FACE_OUTER_BOUND ( 'NONE', #4328, .T. ) ;
#23917 = CARTESIAN_POINT ( 'NONE',  ( 4.000000000000003553, 25.43124999877096926, 6.690598923241489970 ) ) ;
#23918 = CYLINDRICAL_SURFACE ( 'NONE', #17546, 4.000000000000000000 ) ;
#23920 = ORIENTED_EDGE ( 'NONE', *, *, #14777, .F. ) ;
#23919 = DIRECTION ( 'NONE',  ( 0.000000000000000000, 0.000000000000000000, 1.000000000000000000 ) ) ;
#23921 = EDGE_CURVE ( 'NONE', #8698, #4544, #17463, .T. ) ;
#23922 = ORIENTED_EDGE ( 'NONE', *, *, #17341, .T. ) ;
#23923 = VERTEX_POINT ( 'NONE', #15516 ) ;
#23924 = VERTEX_POINT ( 'NONE', #19162 ) ;
#23925 = CARTESIAN_POINT ( 'NONE',  ( -9.110428525061097460, -29.57785765677920509, -6.500000000000000000 ) ) ;
#23926 = DIRECTION ( 'NONE',  ( 1.000000000000000000, 0.000000000000000000, 0.000000000000000000 ) ) ;
#23927 = AXIS2_PLACEMENT_3D ( 'NONE', #9803, #6008, #17782 ) ;
#23928 =( NAMED_UNIT ( * ) PLANE_ANGLE_UNIT ( ) SI_UNIT ( $, .RADIAN. ) );
#23929 = CARTESIAN_POINT ( 'NONE',  ( 6.009258394948636914E-15, 26.15312499938548640, 4.662447845253954171 ) ) ;
#23930 = CIRCLE ( 'NONE', #9322, 3.000000000000000444 ) ;
#23931 = CARTESIAN_POINT ( 'NONE',  ( 2.672651547586948120E-15, -13.33755215474602984, 1.828124999385481786 ) ) ;
#23932 = CARTESIAN_POINT ( 'NONE',  ( -3.999999999999997335, -11.30940107675849404, 3.806249998770963927 ) ) ;
#23933 = CARTESIAN_POINT ( 'NONE',  ( 3.735045420075836212E-15, 27.61562499938548498, 4.662447845253954171 ) ) ;
#23934 = DIRECTION ( 'NONE',  ( 1.000000000000000000, 0.000000000000000000, 0.000000000000000000 ) ) ;
#23935 = CARTESIAN_POINT ( 'NONE',  ( 4.000000000000032863, -11.30940107675847983, 1.706249998770969389 ) ) ;
#23936 = CIRCLE ( 'NONE', #12670, 0.5000000000000002220 ) ;
#23937 = CARTESIAN_POINT ( 'NONE',  ( 3.756430356250003655, 26.04062499938548569, 8.999999999999992895 ) ) ;
#23938 = FACE_OUTER_BOUND ( 'NONE', #24345, .T. ) ;
#23939 = DIRECTION ( 'NONE',  ( 1.000000000000000000, 0.000000000000000000, 0.000000000000000000 ) ) ;
#23940 = FACE_OUTER_BOUND ( 'NONE', #20829, .T. ) ;
#23941 = CARTESIAN_POINT ( 'NONE',  ( -2.000000000000003997, -29.06874999877096855, 5.535898384862238508 ) ) ;
#23942 = CARTESIAN_POINT ( 'NONE',  ( -1.878215178124995832, 28.10312499938548569, 5.746835883940462963 ) ) ;
#23943 = CYLINDRICAL_SURFACE ( 'NONE', #16633, 0.5000000000000004441 ) ;
#23944 = MECHANICAL_DESIGN_GEOMETRIC_PRESENTATION_REPRESENTATION (  '', ( #8495 ), #1396 ) ;
#23945 = CARTESIAN_POINT ( 'NONE',  ( 0.000000000000000000, 0.000000000000000000, -6.500000000000000000 ) ) ;
#23946 = DIRECTION ( 'NONE',  ( 0.000000000000000000, 0.000000000000000000, 1.000000000000000000 ) ) ;
#23947 = ORIENTED_EDGE ( 'NONE', *, *, #5268, .F. ) ;
#23948 = CARTESIAN_POINT ( 'NONE',  ( 2.000000000000000888, 28.52500000000000213, 12.46410161513774817 ) ) ;
#23950 = ORIENTED_EDGE ( 'NONE', *, *, #6026, .T. ) ;
#23949 = CARTESIAN_POINT ( 'NONE',  ( 1.878215178124998497, -29.49062499938548498, 12.25316411605951927 ) ) ;
#23951 = ADVANCED_FACE ( 'NONE', ( #19297 ), #13551, .F. ) ;
#23952 = EDGE_CURVE ( 'NONE', #9729, #24341, #1121, .T. ) ;
#23953 = VERTEX_POINT ( 'NONE', #5306 ) ;
#23954 = CARTESIAN_POINT ( 'NONE',  ( 17.39040739893763643, 20.21883452368375700, 12.46410161513774639 ) ) ;
#23955 = ORIENTED_EDGE ( 'NONE', *, *, #23372, .F. ) ;
#23956 = ORIENTED_EDGE ( 'NONE', *, *, #13095, .T. ) ;
#23957 = ORIENTED_EDGE ( 'NONE', *, *, #14943, .T. ) ;
#23958 = CARTESIAN_POINT ( 'NONE',  ( 20.59759129326749871, 19.08184176541537624, 12.99999999999998757 ) ) ;
#23959 = EDGE_CURVE ( 'NONE', #20975, #7296, #17603, .T. ) ;
#23960 = EDGE_LOOP ( 'NONE', ( #15629, #1592, #20507, #22796 ) ) ;
#23961 = CARTESIAN_POINT ( 'NONE',  ( 2.620986760973688460E-15, 28.48750000000000071, 13.61880215351699874 ) ) ;
#23962 = CARTESIAN_POINT ( 'NONE',  ( -3.756430356249996105, 26.79062499938548569, 6.831223922626973533 ) ) ;
#23963 = ADVANCED_FACE ( 'NONE', ( #9239 ), #7006, .T. ) ;
#23964 = CARTESIAN_POINT ( 'NONE',  ( -1.878215178124998497, -12.25316411605951927, 1.453124999385484228 ) ) ;
#23965 = CARTESIAN_POINT ( 'NONE',  ( 4.648177544792955347E-16, 25.78750000000000497, 12.99999999999999289 ) ) ;
#23966 = CARTESIAN_POINT ( 'NONE',  ( 19.76584424242071947, 19.76584424242064486, 4.662447845253954171 ) ) ;
#23967 =( BOUNDED_CURVE ( )  B_SPLINE_CURVE ( 2, ( #1965, #9929, #2095, #20779, #912, #2736, #22480, #10575, #18573 ),
 .UNSPECIFIED., .F., .F. ) 
 B_SPLINE_CURVE_WITH_KNOTS ( ( 3, 2, 2, 2, 3 ),
 ( 0.6250000000000000000, 0.6333333333333333037, 0.6500000000000000222, 0.6666666666666666297, 0.6750000000000000444 ),
 .UNSPECIFIED. ) 
 CURVE ( )  GEOMETRIC_REPRESENTATION_ITEM ( )  RATIONAL_B_SPLINE_CURVE ( ( 0.9330127018922194093, 0.9330127018922194093, 1.000000000000000000, 0.8660254037844387076, 1.000000000000000000, 0.8660254037844387076, 1.000000000000000000, 0.9330127018922189652, 0.9330127018922194093 ) ) 
 REPRESENTATION_ITEM ( '' )  );
#23968 = CARTESIAN_POINT ( 'NONE',  ( -1.999999999999996669, 27.49374999877097636, 12.46410161513774639 ) ) ;
#23969 = APPLICATION_PROTOCOL_DEFINITION ( 'draft international standard', 'automotive_design', 1998, #21973 ) ;
#23970 = CARTESIAN_POINT ( 'NONE',  ( 4.000000000000003553, 28.60000000000000142, 8.999999999999992895 ) ) ;
#23971 =( BOUNDED_CURVE ( )  B_SPLINE_CURVE ( 2, ( #19457, #15287, #13197, #1817, #21550, #19719, #17263, #7425, #21431 ),
 .UNSPECIFIED., .F., .F. ) 
 B_SPLINE_CURVE_WITH_KNOTS ( ( 3, 2, 2, 2, 3 ),
 ( 0.3250000000000000111, 0.3333333333333333148, 0.3499999999999999778, 0.3666666666666666408, 0.3750000000000000000 ),
 .UNSPECIFIED. ) 
 CURVE ( )  GEOMETRIC_REPRESENTATION_ITEM ( )  RATIONAL_B_SPLINE_CURVE ( ( 0.9330127018922194093, 0.9330127018922196314, 1.000000000000000000, 0.8660254037844387076, 1.000000000000000000, 0.8660254037844387076, 1.000000000000000000, 0.9330127018922194093, 0.9330127018922194093 ) ) 
 REPRESENTATION_ITEM ( '' )  );
#23972 = CARTESIAN_POINT ( 'NONE',  ( -1.999999999999995781, 29.19999999999999929, 5.535898384862237620 ) ) ;
#23973 = DIRECTION ( 'NONE',  ( 0.000000000000000000, 0.000000000000000000, 1.000000000000000000 ) ) ;
#23974 = DIRECTION ( 'NONE',  ( 0.000000000000000000, 0.000000000000000000, 1.000000000000000000 ) ) ;
#23975 = PRESENTATION_LAYER_ASSIGNMENT (  '', '', ( #12709 ) ) ;
#23976 = ORIENTED_EDGE ( 'NONE', *, *, #23130, .F. ) ;
#23977 = ORIENTED_EDGE ( 'NONE', *, *, #17729, .T. ) ;
#23978 = CARTESIAN_POINT ( 'NONE',  ( -3.756430356249996105, 26.41562499938548925, 11.16877607737301226 ) ) ;
#23979 = ORIENTED_EDGE ( 'NONE', *, *, #16566, .F. ) ;
#23980 = DIRECTION ( 'NONE',  ( 0.000000000000000000, 0.000000000000000000, -1.000000000000000000 ) ) ;
#23981 = CARTESIAN_POINT ( 'NONE',  ( -3.756430356249995661, 25.44062499938548427, 6.831223922626973533 ) ) ;
#23982 = CARTESIAN_POINT ( 'NONE',  ( 4.648177544792954952E-15, 28.26250000000000284, 4.999999999999992006 ) ) ;
#23983 = ORIENTED_EDGE ( 'NONE', *, *, #4769, .F. ) ;
#23984 = CARTESIAN_POINT ( 'NONE',  ( 3.999999999999997335, -25.71249999999999503, 11.30940107675849404 ) ) ;
#23985 = VERTEX_POINT ( 'NONE', #25435 ) ;
#23986 = CARTESIAN_POINT ( 'NONE',  ( 0.000000000000000000, 0.000000000000000000, -6.500000000000000000 ) ) ;
#23987 = CARTESIAN_POINT ( 'NONE',  ( 1.878215178125000939, 25.96562499938548285, 12.25316411605952283 ) ) ;
#23988 = CARTESIAN_POINT ( 'NONE',  ( -1.878215178124994722, 29.34062499938548640, 5.746835883940462963 ) ) ;
#23989 = EDGE_CURVE ( 'NONE', #10388, #4038, #21576, .T. ) ;
#23990 = CARTESIAN_POINT ( 'NONE',  ( 6.317933499823220167, -30.45149776762731975, -6.500000000000000000 ) ) ;
#23991 = CARTESIAN_POINT ( 'NONE',  ( -1.499999999999998224, -10.49999999999999289, 30.00000000000000355 ) ) ;
#23992 = CARTESIAN_POINT ( 'NONE',  ( 4.000000000000007105, 29.08750000000000568, 6.690598923241489970 ) ) ;
#23993 = AXIS2_PLACEMENT_3D ( 'NONE', #7786, #15649, #15380 ) ;
#23994 = CARTESIAN_POINT ( 'NONE',  ( 1.878215178125004048, 25.21562499938548285, 5.746835883940462963 ) ) ;
#23995 = FILL_AREA_STYLE_COLOUR ( '', #5832 ) ;
#23996 = CARTESIAN_POINT ( 'NONE',  ( -3.999999999999996447, 27.47499999999999787, 8.999999999999992895 ) ) ;
#23997 = CARTESIAN_POINT ( 'NONE',  ( 18.99023649137219039, 18.99023649137212999, 4.999999999999991118 ) ) ;
#23998 = CARTESIAN_POINT ( 'NONE',  ( 16.62584819264874270, 22.28270244214105134, 11.30940107675849404 ) ) ;
#23999 = LINE ( 'NONE', #6078, #9726 ) ;
#24000 = CARTESIAN_POINT ( 'NONE',  ( 3.959305671612554781E-15, 40.00000000000000000, 12.99999999999999289 ) ) ;
#24001 = DIRECTION ( 'NONE',  ( 0.000000000000000000, 0.000000000000000000, 1.000000000000000000 ) ) ;
#24002 = CARTESIAN_POINT ( 'NONE',  ( 24.86329371854774806, 18.68225429291723216, -2.750000000000000000 ) ) ;
#24003 = CARTESIAN_POINT ( 'NONE',  ( 20.24314131972164077, 20.24314131972156972, 13.33755215474603162 ) ) ;
#24004 = ORIENTED_EDGE ( 'NONE', *, *, #1479, .T. ) ;
#24005 = CARTESIAN_POINT ( 'NONE',  ( -3.999999999999996447, 26.96874999877096712, 8.999999999999992895 ) ) ;
#24006 = EDGE_CURVE ( 'NONE', #17747, #14371, #18024, .T. ) ;
#24007 = CARTESIAN_POINT ( 'NONE',  ( 1.999999999999995781, -27.85000000000000142, 5.535898384862237620 ) ) ;
#24009 = EDGE_LOOP ( 'NONE', ( #20272, #11018, #11819, #2656 ) ) ;
#24008 = CARTESIAN_POINT ( 'NONE',  ( 6.009258394948636914E-15, 27.61562499938548854, 4.662447845253954171 ) ) ;
#24010 = CARTESIAN_POINT ( 'NONE',  ( 1.878215178125000939, 29.22812499938548569, 12.25316411605952283 ) ) ;
#24011 = CARTESIAN_POINT ( 'NONE',  ( -7.734255490827218971, -30.12293631110037140, -6.500000000000000000 ) ) ;
#24012 = CYLINDRICAL_SURFACE ( 'NONE', #5032, 4.000000000000000000 ) ;
#24013 = ORIENTED_EDGE ( 'NONE', *, *, #8865, .F. ) ;
#24014 = ORIENTED_EDGE ( 'NONE', *, *, #460, .F. ) ;
#24015 = DIRECTION ( 'NONE',  ( -0.000000000000000000, -1.000000000000000000, -0.000000000000000000 ) ) ;
#24016 = CARTESIAN_POINT ( 'NONE',  ( -1.878215178124996498, 27.09062499938548996, 5.746835883940462963 ) ) ;
#24017 = DIRECTION ( 'NONE',  ( 0.000000000000000000, 0.000000000000000000, 1.000000000000000000 ) ) ;
#24018 = ADVANCED_FACE ( 'NONE', ( #1395 ), #9096, .T. ) ;
#24019 = CARTESIAN_POINT ( 'NONE',  ( 2.672651547586948120E-15, -13.33755215474603162, 3.628124999385485161 ) ) ;
#24020 = EDGE_CURVE ( 'NONE', #23923, #22016, #5059, .T. ) ;
#24021 = VECTOR ( 'NONE', #21303, 999.9999999999998863 ) ;
#24022 = DIRECTION ( 'NONE',  ( 1.000000000000000000, 0.000000000000000000, 0.000000000000000000 ) ) ;
#24023 = ADVANCED_FACE ( 'NONE', ( #23485 ), #17350, .F. ) ;
#24024 = CARTESIAN_POINT ( 'NONE',  ( 0.000000000000000000, 0.000000000000000000, 20.00000000000000000 ) ) ;
#24025 = CYLINDRICAL_SURFACE ( 'NONE', #17191, 4.000000000000000000 ) ;
#24026 = LINE ( 'NONE', #6106, #10478 ) ;
#24027 = CARTESIAN_POINT ( 'NONE',  ( 7.248980000274197977, 30.24338421796781518, -2.750000000000000000 ) ) ;
#24028 = LINE ( 'NONE', #23520, #21649 ) ;
#24029 = CARTESIAN_POINT ( 'NONE',  ( 18.23893553636149534, 21.06736266110760880, 5.535898384862237620 ) ) ;
#24030 = ORIENTED_EDGE ( 'NONE', *, *, #841, .T. ) ;
#24031 = DIRECTION ( 'NONE',  ( 0.000000000000000000, 0.000000000000000000, -1.000000000000000000 ) ) ;
#24032 = CARTESIAN_POINT ( 'NONE',  ( 3.795382382264993915, 29.75912104221810495, 7.710170883190207824 ) ) ;
#24033 = CARTESIAN_POINT ( 'NONE',  ( -3.756430356249997882, 25.40312499938548285, 11.16877607737301226 ) ) ;
#24034 = CARTESIAN_POINT ( 'NONE',  ( 3.959305739469038251E-15, 30.00000000000000355, 12.99999999999999289 ) ) ;
#24035 = DIRECTION ( 'NONE',  ( 0.000000000000000000, 1.000000000000000000, 0.000000000000000000 ) ) ;
#24036 = DIRECTION ( 'NONE',  ( 0.9297764858882504591, -0.3681245526846803617, 0.000000000000000000 ) ) ;
#24037 = AXIS2_PLACEMENT_3D ( 'NONE', #1239, #17973, #4233 ) ;
#24038 = ORIENTED_EDGE ( 'NONE', *, *, #12740, .T. ) ;
#24039 = CARTESIAN_POINT ( 'NONE',  ( 1.071796769724493226, 26.65134618820330914, 12.99999999999999112 ) ) ;
#24040 = CARTESIAN_POINT ( 'NONE',  ( 3.752267015613588906E-15, 25.50624999877097565, 4.381197846482986158 ) ) ;
#24041 = DIRECTION ( 'NONE',  ( 0.000000000000000000, 0.000000000000000000, 1.000000000000000000 ) ) ;
#24043 = ORIENTED_EDGE ( 'NONE', *, *, #16100, .F. ) ;
#24042 = DIRECTION ( 'NONE',  ( 0.000000000000000000, 0.000000000000000000, -1.000000000000000000 ) ) ;
#24044 = ORIENTED_EDGE ( 'NONE', *, *, #19807, .T. ) ;
#24045 = VERTEX_POINT ( 'NONE', #23105 ) ;
#24046 = EDGE_LOOP ( 'NONE', ( #4785, #21061, #15050, #4230 ) ) ;
#24047 = CARTESIAN_POINT ( 'NONE',  ( 30.12293631110045311, 7.734255490826897450, 1.000000000000000000 ) ) ;
#24048 = CARTESIAN_POINT ( 'NONE',  ( 3.756430356250003211, 26.15312499938548996, 8.999999999999992895 ) ) ;
#24049 = CARTESIAN_POINT ( 'NONE',  ( 3.756430356250004543, 27.87812499938548783, 6.831223922626973533 ) ) ;
#24050 = AXIS2_PLACEMENT_3D ( 'NONE', #19476, #17523, #23926 ) ;
#24051 = CARTESIAN_POINT ( 'NONE',  ( -3.756430356249996994, -8.999999999999992895, 4.415624999385483918 ) ) ;
#24052 = CARTESIAN_POINT ( 'NONE',  ( -3.999999999999996003, -6.690598923241487306, 4.181249998770965703 ) ) ;
#24053 = ADVANCED_FACE ( 'NONE', ( #13426 ), #14992, .F. ) ;
#24054 = CARTESIAN_POINT ( 'NONE',  ( 3.756430356250003655, 25.14062499938548356, 8.999999999999992895 ) ) ;
#24055 = EDGE_CURVE ( 'NONE', #7738, #6126, #20941, .T. ) ;
#24056 = CARTESIAN_POINT ( 'NONE',  ( -28.14012133169333651, -13.24173596767349359, -6.500000000000000000 ) ) ;
#24057 = DIRECTION ( 'NONE',  ( -0.000000000000000000, 0.000000000000000000, 1.000000000000000000 ) ) ;
#24058 = CARTESIAN_POINT ( 'NONE',  ( 3.735045420075836212E-15, 27.05312499938548498, 4.662447845253954171 ) ) ;
#24059 = CYLINDRICAL_SURFACE ( 'NONE', #25089, 4.000000000000000000 ) ;
#24060 = CARTESIAN_POINT ( 'NONE',  ( 3.999999999999996447, -25.61874999877096926, 8.999999999999992895 ) ) ;
#24061 = CARTESIAN_POINT ( 'NONE',  ( 4.000000000000003553, -8.999999999999992895, 0.8437499987709664584 ) ) ;
#24062 = CARTESIAN_POINT ( 'NONE',  ( -3.756430356250003655, -25.25312499938548427, 8.999999999999992895 ) ) ;
#24063 = ADVANCED_FACE ( 'NONE', ( #24928 ), #13038, .F. ) ;
#24064 = CARTESIAN_POINT ( 'NONE',  ( 1.878215178125004048, 28.47812499938548569, 5.746835883940462963 ) ) ;
#24065 = CARTESIAN_POINT ( 'NONE',  ( 1.999999999999998224, -26.20000000000000284, 12.46410161513774639 ) ) ;
#24066 = CARTESIAN_POINT ( 'NONE',  ( 1.859271017917182139E-15, 29.78124999877096712, 12.99999999999999289 ) ) ;
#24067 = DIRECTION ( 'NONE',  ( 0.000000000000000000, -0.000000000000000000, 1.000000000000000000 ) ) ;
#24068 = ORIENTED_EDGE ( 'NONE', *, *, #16370, .T. ) ;
#24069 = CARTESIAN_POINT ( 'NONE',  ( -1.071796769724489451, 26.93259618943234202, 4.999999999999992895 ) ) ;
#24071 = ORIENTED_EDGE ( 'NONE', *, *, #14564, .T. ) ;
#24070 = CARTESIAN_POINT ( 'NONE',  ( -3.756430356250003655, -29.64062499938548356, 8.999999999999992895 ) ) ;
#24072 = EDGE_LOOP ( 'NONE', ( #22767, #18281, #15218, #17284 ) ) ;
#24073 = EDGE_CURVE ( 'NONE', #20170, #23534, #23726, .T. ) ;
#24074 = ORIENTED_EDGE ( 'NONE', *, *, #1842, .T. ) ;
#24075 = EDGE_LOOP ( 'NONE', ( #23979, #4485, #17036, #818 ) ) ;
#24076 = ORIENTED_EDGE ( 'NONE', *, *, #25395, .T. ) ;
#24077 = CARTESIAN_POINT ( 'NONE',  ( -21.28941499438192864, 22.67092431280617859, 1.000000000000000000 ) ) ;
#24078 = ORIENTED_EDGE ( 'NONE', *, *, #2001, .T. ) ;
#24079 = FACE_OUTER_BOUND ( 'NONE', #1108, .T. ) ;
#24080 = CARTESIAN_POINT ( 'NONE',  ( -1.878215178124995832, 27.20312499938548711, 5.746835883940462963 ) ) ;
#24081 = ADVANCED_FACE ( 'NONE', ( #16153 ), #1908, .T. ) ;
#24082 = CARTESIAN_POINT ( 'NONE',  ( -1.878215178124998497, -12.25316411605951927, 1.903124999385483296 ) ) ;
#24083 = DIRECTION ( 'NONE',  ( 0.000000000000000000, 0.000000000000000000, 1.000000000000000000 ) ) ;
#24084 = CARTESIAN_POINT ( 'NONE',  ( 21.41441445718925962, 16.10201970127043936, 6.831223922626973533 ) ) ;
#24085 = DIRECTION ( 'NONE',  ( 0.000000000000000000, -1.000000000000000000, 0.000000000000000000 ) ) ;
#24086 = EDGE_CURVE ( 'NONE', #702, #7351, #14281, .T. ) ;
#24087 = CARTESIAN_POINT ( 'NONE',  ( -18.28012134629613783, -25.16042852506070560, -6.500000000000000000 ) ) ;
#24088 = CARTESIAN_POINT ( 'NONE',  ( 3.756430356250004099, -6.831223922626973533, 1.078124999385482452 ) ) ;
#24089 = CARTESIAN_POINT ( 'NONE',  ( 2.000000000000000888, 27.17500000000000071, 12.46410161513774817 ) ) ;
#24090 = CARTESIAN_POINT ( 'NONE',  ( -3.756430356249997438, 29.00312499938548072, 11.16877607737301048 ) ) ;
#24091 = CARTESIAN_POINT ( 'NONE',  ( -1.999999999999998224, -12.46410161513774639, 3.449999999999998401 ) ) ;
#24092 = DIRECTION ( 'NONE',  ( 0.000000000000000000, 0.000000000000000000, -1.000000000000000000 ) ) ;
#24093 = CARTESIAN_POINT ( 'NONE',  ( 0.000000000000000000, 0.000000000000000000, -6.500000000000000000 ) ) ;
#24094 = ORIENTED_EDGE ( 'NONE', *, *, #11594, .F. ) ;
#24095 = EDGE_LOOP ( 'NONE', ( #14211, #23498, #1501, #4821 ) ) ;
#24096 = CARTESIAN_POINT ( 'NONE',  ( -3.756430356249996549, 25.47812499938548925, 8.999999999999992895 ) ) ;
#24097 = EDGE_CURVE ( 'NONE', #24372, #25585, #3987, .T. ) ;
#24098 = ORIENTED_EDGE ( 'NONE', *, *, #18524, .T. ) ;
#24099 = DIRECTION ( 'NONE',  ( 0.000000000000000000, 0.000000000000000000, 1.000000000000000000 ) ) ;
#24100 = CARTESIAN_POINT ( 'NONE',  ( 3.756430356250003655, 25.25312499938548427, 8.999999999999992895 ) ) ;
#24101 = CARTESIAN_POINT ( 'NONE',  ( 3.756430356250003655, 29.30312499938548498, 8.999999999999992895 ) ) ;
#24102 = CARTESIAN_POINT ( 'NONE',  ( -1.071796769724489895, 28.46740381056767433, 12.99999999999999289 ) ) ;
#24103 = EDGE_LOOP ( 'NONE', ( #12879, #15983, #12788, #18803 ) ) ;
#24104 = CARTESIAN_POINT ( 'NONE',  ( 0.000000000000000000, 0.000000000000000000, -6.500000000000000000 ) ) ;
#24105 = ORIENTED_EDGE ( 'NONE', *, *, #8699, .T. ) ;
#24106 = CARTESIAN_POINT ( 'NONE',  ( -0.2821657309629640453, 38.91194779626417954, 14.58126831647290444 ) ) ;
#24107 =( BOUNDED_CURVE ( )  B_SPLINE_CURVE ( 2, ( #200, #8171, #24111, #4629, #14709, #16806, #6584, #12610, #24504 ),
 .UNSPECIFIED., .F., .F. ) 
 B_SPLINE_CURVE_WITH_KNOTS ( ( 3, 2, 2, 2, 3 ),
 ( 0.3250000000000000111, 0.3333333333333333148, 0.3499999999999999778, 0.3666666666666666408, 0.3750000000000000000 ),
 .UNSPECIFIED. ) 
 CURVE ( )  GEOMETRIC_REPRESENTATION_ITEM ( )  RATIONAL_B_SPLINE_CURVE ( ( 0.9330127018922194093, 0.9330127018922196314, 1.000000000000000000, 0.8660254037844387076, 1.000000000000000000, 0.8660254037844387076, 1.000000000000000000, 0.9330127018922194093, 0.9330127018922194093 ) ) 
 REPRESENTATION_ITEM ( '' )  );
#24108 = CARTESIAN_POINT ( 'NONE',  ( -3.756430356249995661, 28.02812499938548640, 6.831223922626973533 ) ) ;
#24109 = CYLINDRICAL_SURFACE ( 'NONE', #5567, 6.000000000000000888 ) ;
#24110 = CARTESIAN_POINT ( 'NONE',  ( -2.000000000000000888, -26.72500000000000142, 12.46410161513774817 ) ) ;
#24111 = CARTESIAN_POINT ( 'NONE',  ( -1.999999999999996669, 26.50000000000000355, 5.535898384862237620 ) ) ;
#24112 = CARTESIAN_POINT ( 'NONE',  ( -1.999999999999994893, 29.20000000000000284, 5.535898384862237620 ) ) ;
#24113 =( BOUNDED_CURVE ( )  B_SPLINE_CURVE ( 2, ( #17030, #10735, #17164, #813, #18607, #11010, #18721, #5135, #12585 ),
 .UNSPECIFIED., .F., .F. ) 
 B_SPLINE_CURVE_WITH_KNOTS ( ( 3, 2, 2, 2, 3 ),
 ( 0.9250000000000000444, 0.9333333333333333481, 0.9499999999999999556, 0.9666666666666666741, 0.9749999999999999778 ),
 .UNSPECIFIED. ) 
 CURVE ( )  GEOMETRIC_REPRESENTATION_ITEM ( )  RATIONAL_B_SPLINE_CURVE ( ( 0.9330127018922194093, 0.9330127018922198534, 1.000000000000000000, 0.8660254037844387076, 1.000000000000000000, 0.8660254037844387076, 1.000000000000000000, 0.9330127018922194093, 0.9330127018922194093 ) ) 
 REPRESENTATION_ITEM ( '' )  );
#24114 = CARTESIAN_POINT ( 'NONE',  ( 1.878215178125004048, 26.56562499938548427, 5.746835883940462963 ) ) ;
#24115 = CARTESIAN_POINT ( 'NONE',  ( 4.000000000000051514, -11.30940107675846917, 1.256249998770965881 ) ) ;
#24116 = EDGE_CURVE ( 'NONE', #1665, #15816, #1750, .T. ) ;
#24117 = DIRECTION ( 'NONE',  ( -0.000000000000000000, -0.000000000000000000, 1.000000000000000000 ) ) ;
#24118 = DIRECTION ( 'NONE',  ( 1.000000000000000000, 0.000000000000000000, 0.000000000000000000 ) ) ;
#24119 = CARTESIAN_POINT ( 'NONE',  ( 3.878215178125003604, 25.07031249969274356, 8.999999999999992895 ) ) ;
#24120 = CARTESIAN_POINT ( 'NONE',  ( -3.999999999999997335, 29.25624999877096855, 11.30940107675849404 ) ) ;
#24121 = CARTESIAN_POINT ( 'NONE',  ( 5.577813053751546416E-15, 25.33750000000000213, 12.99999999999999289 ) ) ;
#24122 = VECTOR ( 'NONE', #19398, 1000.000000000000000 ) ;
#24123 = CARTESIAN_POINT ( 'NONE',  ( 5.787458694563957451, 38.55544002051694008, 10.35761576072610168 ) ) ;
#24124 = ORIENTED_EDGE ( 'NONE', *, *, #18638, .F. ) ;
#24125 = CARTESIAN_POINT ( 'NONE',  ( -3.999999999999997335, 28.80624999877096926, 11.30940107675849404 ) ) ;
#24126 = CARTESIAN_POINT ( 'NONE',  ( -2.620986760973688460E-15, -29.38749999999999929, 13.61880215351699874 ) ) ;
#24128 = ORIENTED_EDGE ( 'NONE', *, *, #12866, .T. ) ;
#24127 = CARTESIAN_POINT ( 'NONE',  ( 1.878215178125001605, 27.42812499938548854, 12.25316411605952283 ) ) ;
#24129 = CARTESIAN_POINT ( 'NONE',  ( -1.878215178124998497, 28.70312499938548356, 12.25316411605951927 ) ) ;
#24130 = CARTESIAN_POINT ( 'NONE',  ( 7.437084071668728555E-15, 27.13750000000000639, 12.99999999999999112 ) ) ;
#24131 = DIRECTION ( 'NONE',  ( -0.000000000000000000, -0.000000000000000000, 1.000000000000000000 ) ) ;
#24132 = CIRCLE ( 'NONE', #1179, 0.5000000000000004441 ) ;
#24133 = ORIENTED_EDGE ( 'NONE', *, *, #24097, .F. ) ;
#24134 = VERTEX_POINT ( 'NONE', #13800 ) ;
#24135 = CARTESIAN_POINT ( 'NONE',  ( -3.735045420075836212E-15, -25.36562499938548854, 4.662447845253954171 ) ) ;
#24136 = CARTESIAN_POINT ( 'NONE',  ( 4.006172263299091013E-15, 28.40312499938548996, 4.662447845253954171 ) ) ;
#24137 = CYLINDRICAL_SURFACE ( 'NONE', #13879, 0.5000000000000004441 ) ;
#24138 = CARTESIAN_POINT ( 'NONE',  ( -1.878215178124998497, -12.25316411605951927, 3.590624999385481075 ) ) ;
#24139 = VECTOR ( 'NONE', #278, 1000.000000000000000 ) ;
#24140 = DIRECTION ( 'NONE',  ( 0.1253332335642980688, -0.9921147013144785420, 0.000000000000000000 ) ) ;
#24141 = DIRECTION ( 'NONE',  ( 0.000000000000000000, 0.000000000000000000, 1.000000000000000000 ) ) ;
#24142 = CARTESIAN_POINT ( 'NONE',  ( 17.85886564147372724, 23.51571989096603588, 11.30940107675849404 ) ) ;
#24143 = EDGE_CURVE ( 'NONE', #9505, #19523, #14685, .T. ) ;
#24144 = DIRECTION ( 'NONE',  ( 1.000000000000000000, 0.000000000000000000, 0.000000000000000000 ) ) ;
#24145 = CIRCLE ( 'NONE', #9965, 26.00000000000000355 ) ;
#24146 = LINE ( 'NONE', #24635, #21255 ) ;
#24147 = DIRECTION ( 'NONE',  ( -0.7071067811865487940, -0.7071067811865463515, 0.000000000000000000 ) ) ;
#24148 = CARTESIAN_POINT ( 'NONE',  ( 17.50966790313369259, 20.16586528109299437, 5.746835883940462963 ) ) ;
#24149 = CARTESIAN_POINT ( 'NONE',  ( 22.40202671059728345, 16.74517246110483271, 6.690598923241489970 ) ) ;
#24150 = ORIENTED_EDGE ( 'NONE', *, *, #25224, .F. ) ;
#24151 = CYLINDRICAL_SURFACE ( 'NONE', #7200, 31.10000000000000142 ) ;
#24152 = CARTESIAN_POINT ( 'NONE',  ( -0.7500000000000001110, 0.000000000000000000, 17.69999999999999929 ) ) ;
#24153 = CARTESIAN_POINT ( 'NONE',  ( -1.878215178124995832, 25.29062499938548569, 5.746835883940462963 ) ) ;
#24156 = EDGE_CURVE ( 'NONE', #10563, #11374, #21366, .T. ) ;
#24155 = VERTEX_POINT ( 'NONE', #8051 ) ;
#24154 = CARTESIAN_POINT ( 'NONE',  ( -3.999999999999996447, -8.999999999999992895, 2.474999999999997868 ) ) ;
#24157 = CARTESIAN_POINT ( 'NONE',  ( -28.72825533807142051, -11.91206721063020701, 1.000000000000000000 ) ) ;
#24158 = LINE ( 'NONE', #16583, #25500 ) ;
#24159 = ORIENTED_EDGE ( 'NONE', *, *, #17729, .F. ) ;
#24160 = CARTESIAN_POINT ( 'NONE',  ( -3.834746474454188013E-15, -28.26249999999999929, 4.999999999999992006 ) ) ;
#24161 = CARTESIAN_POINT ( 'NONE',  ( 3.752267015613588906E-15, 25.95624999877096784, 4.381197846482986158 ) ) ;
#24162 = CARTESIAN_POINT ( 'NONE',  ( 3.756430356249997882, -27.20312499938548001, 11.16877607737301226 ) ) ;
#24164 = ORIENTED_EDGE ( 'NONE', *, *, #19318, .F. ) ;
#24163 = DIRECTION ( 'NONE',  ( 0.000000000000000000, 0.000000000000000000, 1.000000000000000000 ) ) ;
#24165 = EDGE_CURVE ( 'NONE', #20732, #8492, #4400, .T. ) ;
#24166 = AXIS2_PLACEMENT_3D ( 'NONE', #7569, #17387, #1555 ) ;
#24167 = ORIENTED_EDGE ( 'NONE', *, *, #25293, .F. ) ;
#24168 = VERTEX_POINT ( 'NONE', #13668 ) ;
#24169 = VECTOR ( 'NONE', #19425, 1000.000000000000000 ) ;
#24170 = ADVANCED_FACE ( 'NONE', ( #21638 ), #17853, .F. ) ;
#24171 = ORIENTED_EDGE ( 'NONE', *, *, #11272, .F. ) ;
#24172 = DIRECTION ( 'NONE',  ( 0.000000000000000000, 0.000000000000000000, 1.000000000000000000 ) ) ;
#24173 = CARTESIAN_POINT ( 'NONE',  ( -3.999999999999996447, 26.96874999877096712, 8.999999999999992895 ) ) ;
#24174 = VECTOR ( 'NONE', #12918, 1000.000000000000000 ) ;
#24175 = AXIS2_PLACEMENT_3D ( 'NONE', #13583, #18159, #25610 ) ;
#24176 = CARTESIAN_POINT ( 'NONE',  ( -3.999999999999997335, 26.55624999877096570, 11.30940107675849404 ) ) ;
#24177 = CARTESIAN_POINT ( 'NONE',  ( 3.756430356250004987, 26.49062499938548854, 8.999999999999992895 ) ) ;
#24178 = CARTESIAN_POINT ( 'NONE',  ( -3.999999999999996447, 28.78750000000000497, 6.690598923241487306 ) ) ;
#24179 = CARTESIAN_POINT ( 'NONE',  ( 2.672651547586948120E-15, -13.33755215474602984, 0.5906249993854855163 ) ) ;
#24180 =( LENGTH_UNIT ( ) NAMED_UNIT ( * ) SI_UNIT ( .MILLI., .METRE. ) );
#24181 = CARTESIAN_POINT ( 'NONE',  ( -1.878215178124998497, 26.79062499938548214, 12.25316411605951927 ) ) ;
#24182 = CARTESIAN_POINT ( 'NONE',  ( 0.000000000000000000, 0.000000000000000000, 20.00000000000000000 ) ) ;
#24183 = VECTOR ( 'NONE', #21232, 1000.000000000000000 ) ;
#24184 = DIRECTION ( 'NONE',  ( 0.000000000000000000, -0.000000000000000000, 1.000000000000000000 ) ) ;
#24185 = CARTESIAN_POINT ( 'NONE',  ( -3.756430356249997438, 27.20312499938548356, 11.16877607737301048 ) ) ;
#24186 = CARTESIAN_POINT ( 'NONE',  ( -27.49048467073869517, -14.54246377227329212, -6.500000000000000000 ) ) ;
#24187 = DIRECTION ( 'NONE',  ( -0.1253332335643051187, -0.9921147013144777649, 0.000000000000000000 ) ) ;
#24188 = CARTESIAN_POINT ( 'NONE',  ( 15.35305598651295256, 21.00991023600527186, 11.30940107675849404 ) ) ;
#24189 = CARTESIAN_POINT ( 'NONE',  ( 3.756430356249995661, -25.44062499938548427, 6.831223922626973533 ) ) ;
#24190 = CARTESIAN_POINT ( 'NONE',  ( -23.01025686871661335, -20.92219106202025714, -6.500000000000000000 ) ) ;
#24191 = LINE ( 'NONE', #542, #4518 ) ;
#24192 = ADVANCED_FACE ( 'NONE', ( #25824 ), #3719, .T. ) ;
#24194 = CARTESIAN_POINT ( 'NONE',  ( -9.610428525060479288, 29.57785765677940404, -6.500000000000000000 ) ) ;
#24193 = AXIS2_PLACEMENT_3D ( 'NONE', #19082, #25352, #9409 ) ;
#24195 = CARTESIAN_POINT ( 'NONE',  ( 0.000000000000000000, 0.000000000000000000, -6.500000000000000000 ) ) ;
#24196 = ORIENTED_EDGE ( 'NONE', *, *, #6198, .T. ) ;
#24197 = DIRECTION ( 'NONE',  ( 0.000000000000000000, 0.000000000000000000, -1.000000000000000000 ) ) ;
#24199 = ORIENTED_EDGE ( 'NONE', *, *, #18631, .T. ) ;
#24198 = FACE_OUTER_BOUND ( 'NONE', #8426, .T. ) ;
#24200 = VERTEX_POINT ( 'NONE', #13938 ) ;
#24201 = ORIENTED_EDGE ( 'NONE', *, *, #22730, .F. ) ;
#24202 = EDGE_CURVE ( 'NONE', #5409, #7760, #24726, .T. ) ;
#24203 = ORIENTED_EDGE ( 'NONE', *, *, #4774, .F. ) ;
#24204 = EDGE_LOOP ( 'NONE', ( #13650, #13598, #5117, #16052 ) ) ;
#24205 = CYLINDRICAL_SURFACE ( 'NONE', #9705, 31.10000000000000142 ) ;
#24206 = VECTOR ( 'NONE', #23482, 1000.000000000000000 ) ;
#24207 = EDGE_CURVE ( 'NONE', #17608, #14723, #22221, .T. ) ;
#24208 = AXIS2_PLACEMENT_3D ( 'NONE', #13336, #1167, #10845 ) ;
#24209 = ORIENTED_EDGE ( 'NONE', *, *, #21854, .F. ) ;
#24210 = DIRECTION ( 'NONE',  ( 0.1873813145857189666, -0.9822872507286897203, 0.000000000000000000 ) ) ;
#24211 = CARTESIAN_POINT ( 'NONE',  ( 1.878215178125004048, 25.32812499938548356, 5.746835883940462963 ) ) ;
#24212 = AXIS2_PLACEMENT_3D ( 'NONE', #22378, #10725, #12437 ) ;
#24213 = VECTOR ( 'NONE', #19140, 1000.000000000000000 ) ;
#24214 = CARTESIAN_POINT ( 'NONE',  ( 1.878215178125000939, -12.25316411605952283, 1.528124999385482852 ) ) ;
#24215 = DIRECTION ( 'NONE',  ( 0.000000000000000000, -1.000000000000000000, 0.000000000000000000 ) ) ;
#24216 = CARTESIAN_POINT ( 'NONE',  ( 20.00676625532608455, 17.35056887736664422, 12.25316411605952283 ) ) ;
#24217 = DIRECTION ( 'NONE',  ( 1.000000000000000000, 0.000000000000000000, 0.000000000000000000 ) ) ;
#24218 = DIRECTION ( 'NONE',  ( 0.7705132427757999114, 0.6374239897486768669, 0.000000000000000000 ) ) ;
#24219 = VECTOR ( 'NONE', #23654, 1000.000000000000000 ) ;
#24220 = CARTESIAN_POINT ( 'NONE',  ( 3.735045420075836212E-15, -4.662447845253954171, 1.153124999385480187 ) ) ;
#24221 = CARTESIAN_POINT ( 'NONE',  ( 4.000000000000001776, 29.46250000000000568, 11.30940107675849760 ) ) ;
#24222 = CARTESIAN_POINT ( 'NONE',  ( -1.878215178124998497, 29.49062499938548498, 12.25316411605951927 ) ) ;
#24223 = AXIS2_PLACEMENT_3D ( 'NONE', #24604, #14680, #4749 ) ;
#24224 = CARTESIAN_POINT ( 'NONE',  ( -3.756430356249996105, -6.831223922626973533, 1.340624999385481075 ) ) ;
#24225 = CARTESIAN_POINT ( 'NONE',  ( -1.071796769724487230, 27.38259618943233420, 4.999999999999992006 ) ) ;
#24226 = CARTESIAN_POINT ( 'NONE',  ( 4.000000000000005329, 25.43124999877097636, 6.690598923241489970 ) ) ;
#24227 =( BOUNDED_CURVE ( )  B_SPLINE_CURVE ( 2, ( #7269, #2955, #21007, #12767, #14859, #1113, #14982, #2696, #15247 ),
 .UNSPECIFIED., .F., .F. ) 
 B_SPLINE_CURVE_WITH_KNOTS ( ( 3, 2, 2, 2, 3 ),
 ( 0.1749999999999999889, 0.1833333333333333204, 0.2000000000000000111, 0.2166666666666666741, 0.2250000000000000056 ),
 .UNSPECIFIED. ) 
 CURVE ( )  GEOMETRIC_REPRESENTATION_ITEM ( )  RATIONAL_B_SPLINE_CURVE ( ( 0.9330127018922194093, 0.9330127018922194093, 1.000000000000000000, 0.8660254037844387076, 1.000000000000000000, 0.8660254037844387076, 1.000000000000000000, 0.9330127018922194093, 0.9330127018922194093 ) ) 
 REPRESENTATION_ITEM ( '' )  );
#24228 = ORIENTED_EDGE ( 'NONE', *, *, #14650, .T. ) ;
#24229 = ORIENTED_EDGE ( 'NONE', *, *, #2035, .T. ) ;
#24230 = CARTESIAN_POINT ( 'NONE',  ( 3.756430356250003211, 27.05312499938548854, 8.999999999999992895 ) ) ;
#24231 = AXIS2_PLACEMENT_3D ( 'NONE', #10479, #18478, #21878 ) ;
#24232 = EDGE_LOOP ( 'NONE', ( #11621, #480, #11856, #24381 ) ) ;
#24233 = LINE ( 'NONE', #2525, #12087 ) ;
#24234 = EDGE_CURVE ( 'NONE', #9796, #10164, #3419, .T. ) ;
#24235 = ORIENTED_EDGE ( 'NONE', *, *, #25005, .T. ) ;
#24236 = DIRECTION ( 'NONE',  ( 0.000000000000000000, 0.000000000000000000, 1.000000000000000000 ) ) ;
#24237 = VERTEX_POINT ( 'NONE', #18368 ) ;
#24238 = EDGE_CURVE ( 'NONE', #8387, #9446, #4667, .T. ) ;
#24239 = DIRECTION ( 'NONE',  ( 0.000000000000000000, 0.000000000000000000, 1.000000000000000000 ) ) ;
#24240 = ORIENTED_EDGE ( 'NONE', *, *, #24489, .T. ) ;
#24241 = CARTESIAN_POINT ( 'NONE',  ( 4.000000000000001776, 28.50624999877096855, 11.30940107675849760 ) ) ;
#24242 = CARTESIAN_POINT ( 'NONE',  ( -3.756430356249996994, 26.71562499938548285, 8.999999999999992895 ) ) ;
#24243 = CARTESIAN_POINT ( 'NONE',  ( -5.827558883616271501, -30.54913349766217934, -6.500000000000000000 ) ) ;
#24244 = AXIS2_PLACEMENT_3D ( 'NONE', #23519, #11483, #9656 ) ;
#24245 = VECTOR ( 'NONE', #8342, 1000.000000000000227 ) ;
#24246 = CARTESIAN_POINT ( 'NONE',  ( -27.64012133169333651, -13.24173596767349359, 1.000000000000000000 ) ) ;
#24247 = CARTESIAN_POINT ( 'NONE',  ( 2.000000000000000888, 29.36874999877096926, 12.46410161513774817 ) ) ;
#24248 = CARTESIAN_POINT ( 'NONE',  ( 4.000000000000007105, 28.60000000000000497, 8.999999999999992895 ) ) ;
#24249 = AXIS2_PLACEMENT_3D ( 'NONE', #7810, #25855, #15790 ) ;
#24250 = CARTESIAN_POINT ( 'NONE',  ( -1.878215178124995832, 27.09062499938548640, 5.746835883940462963 ) ) ;
#24251 = CYLINDRICAL_SURFACE ( 'NONE', #11346, 0.5000000000000004441 ) ;
#24252 = AXIS2_PLACEMENT_3D ( 'NONE', #15322, #23290, #8936 ) ;
#24253 = CARTESIAN_POINT ( 'NONE',  ( 17.87212389449003425, 23.52897814398233933, 8.999999999999992895 ) ) ;
#24254 = PRODUCT ( 'bezel locker', 'bezel locker', '', ( #3091 ) ) ;
#24255 = CARTESIAN_POINT ( 'NONE',  ( 6.009258394948636914E-15, 25.95624999877097139, 4.381197846482986158 ) ) ;
#24256 = DIRECTION ( 'NONE',  ( -1.000000000000000000, 0.000000000000000000, 0.000000000000000000 ) ) ;
#24257 = CARTESIAN_POINT ( 'NONE',  ( -3.756430356250003655, -25.14062499938548356, 8.999999999999992895 ) ) ;
#24258 = AXIS2_PLACEMENT_3D ( 'NONE', #913, #14510, #6917 ) ;
#24259 = CARTESIAN_POINT ( 'NONE',  ( 17.75721904254721295, 17.75721904254714545, 4.999999999999992006 ) ) ;
#24260 = ORIENTED_EDGE ( 'NONE', *, *, #14610, .F. ) ;
#24261 = CARTESIAN_POINT ( 'NONE',  ( 4.000000000000003553, 26.78124999877097068, 6.690598923241489970 ) ) ;
#24262 = CARTESIAN_POINT ( 'NONE',  ( -4.000000000000003553, -28.63750000000000284, 6.690598923241489970 ) ) ;
#24264 = VERTEX_POINT ( 'NONE', #2678 ) ;
#24263 = CARTESIAN_POINT ( 'NONE',  ( 0.000000000000000000, 28.29062499938549280, 13.33755215474603162 ) ) ;
#24265 = EDGE_CURVE ( 'NONE', #7323, #17107, #4890, .T. ) ;
#24266 = VERTEX_POINT ( 'NONE', #597 ) ;
#24267 = CARTESIAN_POINT ( 'NONE',  ( -14.48253926456356666, -27.25313774936403988, -6.500000000000000000 ) ) ;
#24268 = AXIS2_PLACEMENT_3D ( 'NONE', #873, #20343, #498 ) ;
#24269 = CARTESIAN_POINT ( 'NONE',  ( -1.999999999999996669, -8.999999999999992895, 8.000000000000000000 ) ) ;
#24270 = CARTESIAN_POINT ( 'NONE',  ( -3.999999999999997335, 25.65624999877097068, 11.30940107675849404 ) ) ;
#24271 = ORIENTED_EDGE ( 'NONE', *, *, #21368, .T. ) ;
#24272 = ORIENTED_EDGE ( 'NONE', *, *, #11052, .F. ) ;
#24273 = CARTESIAN_POINT ( 'NONE',  ( 3.756430356249997438, -27.31562499938548427, 11.16877607737301048 ) ) ;
#24274 = CARTESIAN_POINT ( 'NONE',  ( 1.878215178125001605, 29.11562499938549209, 12.25316411605952283 ) ) ;
#24275 =( BOUNDED_CURVE ( )  B_SPLINE_CURVE ( 2, ( #22209, #20235, #12661, #10414, #2331, #18413, #14374, #10291, #371 ),
 .UNSPECIFIED., .F., .F. ) 
 B_SPLINE_CURVE_WITH_KNOTS ( ( 3, 2, 2, 2, 3 ),
 ( 0.6250000000000000000, 0.6333333333333333037, 0.6500000000000000222, 0.6666666666666666297, 0.6750000000000000444 ),
 .UNSPECIFIED. ) 
 CURVE ( )  GEOMETRIC_REPRESENTATION_ITEM ( )  RATIONAL_B_SPLINE_CURVE ( ( 0.9330127018922194093, 0.9330127018922194093, 1.000000000000000000, 0.8660254037844387076, 1.000000000000000000, 0.8660254037844387076, 1.000000000000000000, 0.9330127018922189652, 0.9330127018922194093 ) ) 
 REPRESENTATION_ITEM ( '' )  );
#24276 = CARTESIAN_POINT ( 'NONE',  ( -3.110308778861381462, 38.49999999999999289, 3.869115154270378554 ) ) ;
#24277 = ADVANCED_FACE ( 'NONE', ( #16424 ), #24251, .F. ) ;
#24278 = VECTOR ( 'NONE', #3713, 1000.000000000000000 ) ;
#24279 = DIRECTION ( 'NONE',  ( 0.000000000000000000, 0.000000000000000000, 1.000000000000000000 ) ) ;
#24280 = AXIS2_PLACEMENT_3D ( 'NONE', #21910, #23732, #3992 ) ;
#24281 = VECTOR ( 'NONE', #23251, 1000.000000000000000 ) ;
#24282 = ADVANCED_FACE ( 'NONE', ( #10248 ), #4373, .T. ) ;
#24283 = CYLINDRICAL_SURFACE ( 'NONE', #22554, 0.5000000000000004441 ) ;
#24284 = CARTESIAN_POINT ( 'NONE',  ( 3.469446951953614189E-15, 39.50000000000000000, 8.999999999999992895 ) ) ;
#24285 = AXIS2_PLACEMENT_3D ( 'NONE', #17502, #13201, #13468 ) ;
#24286 = LINE ( 'NONE', #6884, #2560 ) ;
#24287 = CARTESIAN_POINT ( 'NONE',  ( 20.09187391231935393, 18.57612438446723857, 4.999999999999992895 ) ) ;
#24288 = CARTESIAN_POINT ( 'NONE',  ( 1.071796769724494336, 25.35759618943234628, 12.99999999999999467 ) ) ;
#24289 = CARTESIAN_POINT ( 'NONE',  ( 19.79463422097012426, 17.13843684301067682, 5.746835883940462963 ) ) ;
#24290 = CARTESIAN_POINT ( 'NONE',  ( 22.08382865906333947, 16.42697440957088872, 6.690598923241489970 ) ) ;
#24291 = ORIENTED_EDGE ( 'NONE', *, *, #25796, .F. ) ;
#24292 = CARTESIAN_POINT ( 'NONE',  ( -27.92360179968386547, -13.69242354489123770, -6.500000000000000000 ) ) ;
#24293 = CARTESIAN_POINT ( 'NONE',  ( 5.208121455455055226, 38.94679493378507118, 7.072325123572092309 ) ) ;
#24294 = CARTESIAN_POINT ( 'NONE',  ( -3.756430356249996994, 25.81562499938548427, 8.999999999999992895 ) ) ;
#24296 = EDGE_LOOP ( 'NONE', ( #1145, #17303, #157, #11112 ) ) ;
#24295 = LINE ( 'NONE', #506, #10786 ) ;
#24297 = CIRCLE ( 'NONE', #20106, 6.000000000000000000 ) ;
#24298 = CARTESIAN_POINT ( 'NONE',  ( -3.999999999999996447, -8.999999999999992895, 0.2249999999999995060 ) ) ;
#24299 = EDGE_LOOP ( 'NONE', ( #23683, #4193, #9887, #21725 ) ) ;
#24300 = FACE_OUTER_BOUND ( 'NONE', #20702, .T. ) ;
#24301 = FACE_OUTER_BOUND ( 'NONE', #12426, .T. ) ;
#24302 = CARTESIAN_POINT ( 'NONE',  ( -3.756430356250003655, -27.39062499938548356, 8.999999999999992895 ) ) ;
#24304 = EDGE_LOOP ( 'NONE', ( #12519, #22463, #22307, #25142 ) ) ;
#24303 = FACE_OUTER_BOUND ( 'NONE', #18291, .T. ) ;
#24305 = CIRCLE ( 'NONE', #13868, 31.10000000000000142 ) ;
#24306 = AXIS2_PLACEMENT_3D ( 'NONE', #12721, #16779, #299 ) ;
#24307 = ORIENTED_EDGE ( 'NONE', *, *, #24390, .T. ) ;
#24308 = CARTESIAN_POINT ( 'NONE',  ( -3.756430356250004099, -25.17812499938548498, 6.831223922626973533 ) ) ;
#24309 = ORIENTED_EDGE ( 'NONE', *, *, #4746, .T. ) ;
#24310 = EDGE_LOOP ( 'NONE', ( #24403, #14249, #960, #13244 ) ) ;
#24312 = CARTESIAN_POINT ( 'NONE',  ( -1.878215178124999829, 26.45312499938549422, 12.25316411605951927 ) ) ;
#24311 = AXIS2_PLACEMENT_3D ( 'NONE', #16577, #22848, #12653 ) ;
#24313 = EDGE_CURVE ( 'NONE', #1345, #7996, #10093, .T. ) ;
#24314 =( NAMED_UNIT ( * ) PLANE_ANGLE_UNIT ( ) SI_UNIT ( $, .RADIAN. ) );
#24315 = EDGE_CURVE ( 'NONE', #22640, #14520, #7084, .T. ) ;
#24316 = CIRCLE ( 'NONE', #13889, 0.4999999999999997224 ) ;
#24317 = ADVANCED_FACE ( 'NONE', ( #16813 ), #12470, .T. ) ;
#24318 = DIRECTION ( 'NONE',  ( 0.000000000000000000, 1.000000000000000000, 0.000000000000000000 ) ) ;
#24319 = CARTESIAN_POINT ( 'NONE',  ( -1.878215178124995832, -5.746835883940462963, 3.103124999385483029 ) ) ;
#24320 = VECTOR ( 'NONE', #5465, 1000.000000000000000 ) ;
#24321 = CARTESIAN_POINT ( 'NONE',  ( 3.756430356250004099, 26.07812499938548356, 6.831223922626973533 ) ) ;
#24322 = AXIS2_PLACEMENT_3D ( 'NONE', #22093, #538, #8511 ) ;
#24323 = DIRECTION ( 'NONE',  ( 0.000000000000000000, 0.000000000000000000, 1.000000000000000000 ) ) ;
#24324 = FACE_OUTER_BOUND ( 'NONE', #1080, .T. ) ;
#24325 = CARTESIAN_POINT ( 'NONE',  ( 1.878215178125004048, 27.46562499938548640, 5.746835883940462963 ) ) ;
#24326 = FACE_OUTER_BOUND ( 'NONE', #12761, .T. ) ;
#24328 = EDGE_CURVE ( 'NONE', #855, #12364, #20538, .T. ) ;
#24327 = CARTESIAN_POINT ( 'NONE',  ( 2.000000000000003997, 25.91874999877096997, 5.535898384862238508 ) ) ;
#24329 = DIRECTION ( 'NONE',  ( -0.000000000000000000, 1.000000000000000000, -0.000000000000000000 ) ) ;
#24330 = CARTESIAN_POINT ( 'NONE',  ( -4.000000000000003553, -28.13124999877096855, 6.690598923241489970 ) ) ;
#24331 = CARTESIAN_POINT ( 'NONE',  ( -22.67092431280563503, 21.28941499438250062, -6.500000000000000000 ) ) ;
#24332 = CARTESIAN_POINT ( 'NONE',  ( -3.999999999999996447, 27.92500000000000071, 8.999999999999992895 ) ) ;
#24333 = CYLINDRICAL_SURFACE ( 'NONE', #1642, 31.10000000000000142 ) ;
#24334 = LINE ( 'NONE', #8634, #15576 ) ;
#24335 = ORIENTED_EDGE ( 'NONE', *, *, #2728, .T. ) ;
#24336 = DIRECTION ( 'NONE',  ( 1.000000000000000000, 0.000000000000000000, 0.000000000000000000 ) ) ;
#24338 = ORIENTED_EDGE ( 'NONE', *, *, #16167, .F. ) ;
#24337 = CARTESIAN_POINT ( 'NONE',  ( 16.23990935651717393, 26.52310962334745170, -6.500000000000000000 ) ) ;
#24339 = AXIS2_PLACEMENT_3D ( 'NONE', #24047, #8227, #134 ) ;
#24340 = ORIENTED_EDGE ( 'NONE', *, *, #13667, .F. ) ;
#24341 = VERTEX_POINT ( 'NONE', #24391 ) ;
#24342 = ORIENTED_EDGE ( 'NONE', *, *, #10353, .F. ) ;
#24343 = EDGE_CURVE ( 'NONE', #18977, #1175, #7769, .T. ) ;
#24344 = ORIENTED_EDGE ( 'NONE', *, *, #6636, .T. ) ;
#24345 = EDGE_LOOP ( 'NONE', ( #7257, #18728, #9676, #11619 ) ) ;
#24346 = DIRECTION ( 'NONE',  ( -0.7289686274214034478, 0.6845471059286972748, 0.000000000000000000 ) ) ;
#24347 = ORIENTED_EDGE ( 'NONE', *, *, #9292, .F. ) ;
#24348 = CARTESIAN_POINT ( 'NONE',  ( 4.000000000000003553, 29.05000000000000071, 8.999999999999992895 ) ) ;
#24349 = CARTESIAN_POINT ( 'NONE',  ( -1.878215178124998497, 25.55312499938548854, 12.25316411605951927 ) ) ;
#24350 = EDGE_CURVE ( 'NONE', #18321, #9729, #20121, .T. ) ;
#24351 = CIRCLE ( 'NONE', #2233, 1.000000000000000000 ) ;
#24352 = CARTESIAN_POINT ( 'NONE',  ( 3.756430356250003655, -8.999999999999992895, 1.603124999385485028 ) ) ;
#24353 = CARTESIAN_POINT ( 'NONE',  ( -3.999999999999996447, -8.999999999999992895, 1.518749998770968501 ) ) ;
#24354 = CARTESIAN_POINT ( 'NONE',  ( 17.16267987305034382, 22.47507462896901842, 6.831223922626973533 ) ) ;
#24355 = EDGE_CURVE ( 'NONE', #3025, #24553, #7879, .T. ) ;
#24356 =( BOUNDED_SURFACE ( )  B_SPLINE_SURFACE ( 1, 2, ( 
 ( #9301, #17287, #25367, #7330, #21325, #9422, #23544, #7717, #15437, #25120, #17403, #3535, #11506, #19477, #21573, #3652, #25636, #14597, #15820, #2699, #139, #8705, #14738, #12149, #735, #6749, #6133, #23929, #2226, #16692, #8112, #19860, #17909, #17787, #10659, #10056, #24177, #24662, #15960, #3921, #22715, #21963, #4660, #7975, #18651, #20124, #25876, #6011, #4795, #10183, #1843, #1959, #22083, #19744, #19984, #4041, #22580, #9806, #9922, #23790, #13992, #12642, #12008, #25753, #7836, #5880, #2088, #13864, #21839, #20614, #264, #18055, #16087, #24049, #14118, #4170, #6609, #18182, #8230, #11891, #16206, #5049, #20867, #867, #1116, #7001, #1389, #3088, #7389, #6879, #15369, #7274, #10924, #14985, #7140, #19035, #25190, #9091, #13279, #14863, #19290, #24923, #11054, #24798, #1000, #22962, #9231, #15250, #17078, #25052, #2960, #17219, #21127, #3334, #9363, #13032, #23216, #15127, #21251, #5300, #11311 ),
 ( #12889, #17347, #25311, #20742, #11172, #23102, #5185, #23339, #18916, #12771, #8981, #8847, #2819, #16957, #13160, #21011, #10782, #3204, #19155, #18778, #1248, #16835, #22837, #4911, #19803, #16028, #11565, #1511, #13797, #19533, #11698, #23477, #21393, #9989, #21772, #2022, #17458, #1633, #3714, #19416, #25429, #11446, #25570, #9611, #17983, #23721, #3857, #25819, #7516, #7901, #5430, #15510, #7778, #19675, #9480, #13419, #5564, #13548, #17725, #73, #15757, #3473, #1903, #21511, #25696, #5810, #11833, #8047, #3592, #17593, #1778, #7652, #15639, #23605, #9866, #11950, #9745, #5683, #13662, #21635, #17849, #15892, #23864, #5949, #13935, #21903, #3984, #19920, #8294, #4103, #2405, #22158, #16151, #20188, #2159, #4241, #24248, #22291, #8172, #14451, #22548, #10364, #12081, #322, #14568, #6464, #8433, #12220, #16279, #23992, #2539, #6074, #24112, #20056, #8680, #20312, #4630, #18363, #14186, #20441, #14057 ) ),
 .UNSPECIFIED., .F., .F., .F. ) 
 B_SPLINE_SURFACE_WITH_KNOTS ( ( 2, 2 ),
 ( 3, 2, 2, 2, 2, 2, 2, 2, 2, 2, 2, 2, 2, 2, 2, 2, 2, 2, 2, 2, 2, 2, 2, 2, 2, 2, 2, 2, 2, 2, 2, 2, 2, 2, 2, 2, 2, 2, 2, 2, 2, 2, 2, 2, 2, 2, 2, 2, 2, 2, 2, 2, 2, 2, 2, 2, 2, 2, 2, 2, 3 ),
 ( 0.000000000000000000, 1.000000000000000000 ),
 ( 0.000000000000000000, 0.01666666666666666644, 0.03333333333333333287, 0.05000000000000000278, 0.06666666666666666574, 0.08333333333333332871, 0.1000000000000000056, 0.1166666666666666685, 0.1333333333333333315, 0.1499999999999999944, 0.1666666666666666574, 0.1833333333333333204, 0.2000000000000000111, 0.2166666666666666741, 0.2333333333333333370, 0.2500000000000000000, 0.2666666666666666630, 0.2833333333333333259, 0.2999999999999999889, 0.3166666666666666519, 0.3333333333333333148, 0.3499999999999999778, 0.3666666666666666408, 0.3833333333333333592, 0.4000000000000000222, 0.4166666666666666852, 0.4333333333333333481, 0.4500000000000000111, 0.4666666666666666741, 0.4833333333333333370, 0.5000000000000000000, 0.5166666666666667185, 0.5333333333333333259, 0.5500000000000000444, 0.5666666666666666519, 0.5833333333333333703, 0.5999999999999999778, 0.6166666666666666963, 0.6333333333333333037, 0.6500000000000000222, 0.6666666666666666297, 0.6833333333333333481, 0.6999999999999999556, 0.7166666666666666741, 0.7333333333333332815, 0.7500000000000000000, 0.7666666666666667185, 0.7833333333333333259, 0.8000000000000000444, 0.8166666666666666519, 0.8333333333333333703, 0.8499999999999999778, 0.8666666666666666963, 0.8833333333333333037, 0.9000000000000000222, 0.9166666666666666297, 0.9333333333333333481, 0.9499999999999999556, 0.9666666666666666741, 0.9833333333333332815, 1.000000000000000000 ),
 .UNSPECIFIED. ) 
 GEOMETRIC_REPRESENTATION_ITEM ( )  RATIONAL_B_SPLINE_SURFACE ( (
 ( 1.000000000000000000, 0.8660254037844387076, 1.000000000000000000, 0.8660254037844387076, 1.000000000000000000, 0.8660254037844387076, 1.000000000000000000, 0.8660254037844387076, 1.000000000000000000, 0.8660254037844387076, 1.000000000000000000, 0.8660254037844387076, 1.000000000000000000, 0.8660254037844387076, 1.000000000000000000, 0.8660254037844387076, 1.000000000000000000, 0.8660254037844387076, 1.000000000000000000, 0.8660254037844387076, 1.000000000000000000, 0.8660254037844387076, 1.000000000000000000, 0.8660254037844387076, 1.000000000000000000, 0.8660254037844387076, 1.000000000000000000, 0.8660254037844387076, 1.000000000000000000, 0.8660254037844387076, 1.000000000000000000, 0.8660254037844387076, 1.000000000000000000, 0.8660254037844387076, 1.000000000000000000, 0.8660254037844387076, 1.000000000000000000, 0.8660254037844387076, 1.000000000000000000, 0.8660254037844387076, 1.000000000000000000, 0.8660254037844387076, 1.000000000000000000, 0.8660254037844387076, 1.000000000000000000, 0.8660254037844387076, 1.000000000000000000, 0.8660254037844387076, 1.000000000000000000, 0.8660254037844387076, 1.000000000000000000, 0.8660254037844387076, 1.000000000000000000, 0.8660254037844387076, 1.000000000000000000, 0.8660254037844387076, 1.000000000000000000, 0.8660254037844387076, 1.000000000000000000, 0.8660254037844387076, 1.000000000000000000, 0.8660254037844387076, 1.000000000000000000, 0.8660254037844387076, 1.000000000000000000, 0.8660254037844387076, 1.000000000000000000, 0.8660254037844387076, 1.000000000000000000, 0.8660254037844387076, 1.000000000000000000, 0.8660254037844387076, 1.000000000000000000, 0.8660254037844387076, 1.000000000000000000, 0.8660254037844387076, 1.000000000000000000, 0.8660254037844387076, 1.000000000000000000, 0.8660254037844387076, 1.000000000000000000, 0.8660254037844387076, 1.000000000000000000, 0.8660254037844387076, 1.000000000000000000, 0.8660254037844387076, 1.000000000000000000, 0.8660254037844387076, 1.000000000000000000, 0.8660254037844387076, 1.000000000000000000, 0.8660254037844387076, 1.000000000000000000, 0.8660254037844387076, 1.000000000000000000, 0.8660254037844387076, 1.000000000000000000, 0.8660254037844387076, 1.000000000000000000, 0.8660254037844387076, 1.000000000000000000, 0.8660254037844387076, 1.000000000000000000, 0.8660254037844387076, 1.000000000000000000, 0.8660254037844387076, 1.000000000000000000, 0.8660254037844387076, 1.000000000000000000, 0.8660254037844387076, 1.000000000000000000, 0.8660254037844387076, 1.000000000000000000, 0.8660254037844387076, 1.000000000000000000, 0.8660254037844387076, 1.000000000000000000, 0.8660254037844387076, 1.000000000000000000, 0.8660254037844387076, 1.000000000000000000),
 ( 1.000000000000000000, 0.8660254037844387076, 1.000000000000000000, 0.8660254037844387076, 1.000000000000000000, 0.8660254037844387076, 1.000000000000000000, 0.8660254037844387076, 1.000000000000000000, 0.8660254037844387076, 1.000000000000000000, 0.8660254037844387076, 1.000000000000000000, 0.8660254037844387076, 1.000000000000000000, 0.8660254037844387076, 1.000000000000000000, 0.8660254037844387076, 1.000000000000000000, 0.8660254037844387076, 1.000000000000000000, 0.8660254037844387076, 1.000000000000000000, 0.8660254037844387076, 1.000000000000000000, 0.8660254037844387076, 1.000000000000000000, 0.8660254037844387076, 1.000000000000000000, 0.8660254037844387076, 1.000000000000000000, 0.8660254037844387076, 1.000000000000000000, 0.8660254037844387076, 1.000000000000000000, 0.8660254037844387076, 1.000000000000000000, 0.8660254037844387076, 1.000000000000000000, 0.8660254037844387076, 1.000000000000000000, 0.8660254037844387076, 1.000000000000000000, 0.8660254037844387076, 1.000000000000000000, 0.8660254037844387076, 1.000000000000000000, 0.8660254037844387076, 1.000000000000000000, 0.8660254037844387076, 1.000000000000000000, 0.8660254037844387076, 1.000000000000000000, 0.8660254037844387076, 1.000000000000000000, 0.8660254037844387076, 1.000000000000000000, 0.8660254037844387076, 1.000000000000000000, 0.8660254037844387076, 1.000000000000000000, 0.8660254037844387076, 1.000000000000000000, 0.8660254037844387076, 1.000000000000000000, 0.8660254037844387076, 1.000000000000000000, 0.8660254037844387076, 1.000000000000000000, 0.8660254037844387076, 1.000000000000000000, 0.8660254037844387076, 1.000000000000000000, 0.8660254037844387076, 1.000000000000000000, 0.8660254037844387076, 1.000000000000000000, 0.8660254037844387076, 1.000000000000000000, 0.8660254037844387076, 1.000000000000000000, 0.8660254037844387076, 1.000000000000000000, 0.8660254037844387076, 1.000000000000000000, 0.8660254037844387076, 1.000000000000000000, 0.8660254037844387076, 1.000000000000000000, 0.8660254037844387076, 1.000000000000000000, 0.8660254037844387076, 1.000000000000000000, 0.8660254037844387076, 1.000000000000000000, 0.8660254037844387076, 1.000000000000000000, 0.8660254037844387076, 1.000000000000000000, 0.8660254037844387076, 1.000000000000000000, 0.8660254037844387076, 1.000000000000000000, 0.8660254037844387076, 1.000000000000000000, 0.8660254037844387076, 1.000000000000000000, 0.8660254037844387076, 1.000000000000000000, 0.8660254037844387076, 1.000000000000000000, 0.8660254037844387076, 1.000000000000000000, 0.8660254037844387076, 1.000000000000000000, 0.8660254037844387076, 1.000000000000000000, 0.8660254037844387076, 1.000000000000000000, 0.8660254037844387076, 1.000000000000000000) ) ) 
 REPRESENTATION_ITEM ( '' )  SURFACE ( )  );
#24357 = CYLINDRICAL_SURFACE ( 'NONE', #18841, 0.5000000000000004441 ) ;
#24358 = AXIS2_PLACEMENT_3D ( 'NONE', #11944, #13658, #6069 ) ;
#24359 =( NAMED_UNIT ( * ) SI_UNIT ( $, .STERADIAN. ) SOLID_ANGLE_UNIT ( ) );
#24360 = CARTESIAN_POINT ( 'NONE',  ( 3.756430356250002323, -11.16877607737301226, 1.903124999385483740 ) ) ;
#24362 = ADVANCED_FACE ( 'NONE', ( #21497 ), #5785, .T. ) ;
#24361 = CARTESIAN_POINT ( 'NONE',  ( 3.834746474454188013E-15, 27.75624999877096855, 4.999999999999992006 ) ) ;
#24363 = CARTESIAN_POINT ( 'NONE',  ( 25.45105997952917676, 17.87326343783944083, 1.000000000000000000 ) ) ;
#24364 = CARTESIAN_POINT ( 'NONE',  ( 1.878215178125000939, 29.56562499938548427, 12.25316411605952283 ) ) ;
#24365 = EDGE_CURVE ( 'NONE', #2838, #16618, #21613, .T. ) ;
#24366 = CARTESIAN_POINT ( 'NONE',  ( 1.878215178125000939, -12.25316411605952283, 2.878124999385483385 ) ) ;
#24367 = CARTESIAN_POINT ( 'NONE',  ( 3.834746474454188013E-15, 26.01249999999999574, 4.999999999999992006 ) ) ;
#24368 = CARTESIAN_POINT ( 'NONE',  ( -4.000000000000003553, -28.18750000000000000, 6.690598923241489970 ) ) ;
#24369 = VERTEX_POINT ( 'NONE', #49 ) ;
#24370 = ORIENTED_EDGE ( 'NONE', *, *, #23291, .T. ) ;
#24371 = CARTESIAN_POINT ( 'NONE',  ( 0.000000000000000000, 28.29062499938548925, 13.33755215474602984 ) ) ;
#24372 = VERTEX_POINT ( 'NONE', #3965 ) ;
#24373 = CARTESIAN_POINT ( 'NONE',  ( 3.959305671612554781E-15, 30.00000000000000355, 12.99999999999999289 ) ) ;
#24374 =( GEOMETRIC_REPRESENTATION_CONTEXT ( 3 ) GLOBAL_UNCERTAINTY_ASSIGNED_CONTEXT ( ( #774 ) ) GLOBAL_UNIT_ASSIGNED_CONTEXT ( ( #11385, #11509, #3655 ) ) REPRESENTATION_CONTEXT ( 'NONE', 'WORKASPACE' ) );
#24375 = VERTEX_POINT ( 'NONE', #11930 ) ;
#24376 = CARTESIAN_POINT ( 'NONE',  ( 4.000000000000003553, -8.999999999999992895, 2.193749998770967213 ) ) ;
#24377 = ORIENTED_EDGE ( 'NONE', *, *, #21628, .F. ) ;
#24378 = DIRECTION ( 'NONE',  ( 0.000000000000000000, 0.000000000000000000, 1.000000000000000000 ) ) ;
#24379 = VECTOR ( 'NONE', #23509, 1000.000000000000000 ) ;
#24380 = DIRECTION ( 'NONE',  ( 0.000000000000000000, 0.000000000000000000, 1.000000000000000000 ) ) ;
#24381 = ORIENTED_EDGE ( 'NONE', *, *, #24207, .T. ) ;
#24382 = CARTESIAN_POINT ( 'NONE',  ( 4.000000000000003553, 28.58124999877096784, 6.690598923241489970 ) ) ;
#24383 = CARTESIAN_POINT ( 'NONE',  ( -3.756430356249997882, 26.30312499938548498, 11.16877607737301226 ) ) ;
#24384 = DIRECTION ( 'NONE',  ( -0.000000000000000000, -1.000000000000000000, -0.000000000000000000 ) ) ;
#24385 = LINE ( 'NONE', #8814, #20945 ) ;
#24386 = DIRECTION ( 'NONE',  ( -0.000000000000000000, -0.000000000000000000, 1.000000000000000000 ) ) ;
#24387 = CARTESIAN_POINT ( 'NONE',  ( 20.51285331117640709, 15.20045855525759393, 8.999999999999992895 ) ) ;
#24388 = EDGE_CURVE ( 'NONE', #23620, #22640, #17628, .T. ) ;
#24389 = CARTESIAN_POINT ( 'NONE',  ( 3.756430356250002323, 28.25312499938548427, 11.16877607737301226 ) ) ;
#24390 = EDGE_CURVE ( 'NONE', #1927, #2390, #12197, .T. ) ;
#24391 = CARTESIAN_POINT ( 'NONE',  ( -1.453535542772161238, 31.06601413805604750, -6.500000000000000000 ) ) ;
#24392 = CARTESIAN_POINT ( 'NONE',  ( 23.02516456238698694, 17.36831031289452909, 11.30940107675849760 ) ) ;
#24393 = CARTESIAN_POINT ( 'NONE',  ( 0.7500000000000000000, 0.000000000000000000, 18.19999999999999929 ) ) ;
#24394 = ADVANCED_FACE ( 'NONE', ( #20921 ), #12941, .F. ) ;
#24395 = CYLINDRICAL_SURFACE ( 'NONE', #17651, 0.5000000000000001110 ) ;
#24396 = CARTESIAN_POINT ( 'NONE',  ( -3.756430356250003211, -25.17812499938548498, 6.831223922626973533 ) ) ;
#24397 = LINE ( 'NONE', #8688, #21285 ) ;
#24398 = ORIENTED_EDGE ( 'NONE', *, *, #6565, .T. ) ;
#24399 = CARTESIAN_POINT ( 'NONE',  ( 3.756430356250004099, 25.74062499938548143, 6.831223922626973533 ) ) ;
#24400 = CARTESIAN_POINT ( 'NONE',  ( -4.000000000000003553, -28.60000000000000142, 8.999999999999992895 ) ) ;
#24402 = VERTEX_POINT ( 'NONE', #14428 ) ;
#24401 = CARTESIAN_POINT ( 'NONE',  ( -1.878215178124996498, 28.55312499938548854, 5.746835883940462963 ) ) ;
#24403 = ORIENTED_EDGE ( 'NONE', *, *, #16826, .T. ) ;
#24404 = DIRECTION ( 'NONE',  ( -0.000000000000000000, -1.000000000000000000, -0.000000000000000000 ) ) ;
#24405 = EDGE_LOOP ( 'NONE', ( #19437, #24468, #10144, #15433 ) ) ;
#24406 = DIRECTION ( 'NONE',  ( 0.7705132427757873659, -0.6374239897486919659, 0.000000000000000000 ) ) ;
#24407 = DIRECTION ( 'NONE',  ( -0.000000000000000000, -1.000000000000000000, -0.000000000000000000 ) ) ;
#24408 = EDGE_LOOP ( 'NONE', ( #14430, #22540, #705, #6119 ) ) ;
#24409 = EDGE_LOOP ( 'NONE', ( #7252, #21109, #20860, #16331, #281, #550, #2272, #10629, #19854, #183, #9733, #21094, #9667, #5080, #9296, #22642, #21446, #4548, #15356, #2777, #11498, #16644, #4695, #23205, #4851, #2341, #610, #12456, #11828, #4846, #17383, #11973, #21442, #23156, #25678, #14344, #8915, #24618, #9210, #14794, #13790, #3700, #21828, #7881, #2526, #4084, #8881, #14286, #15277, #886, #24585, #23088, #14095, #10415, #575, #16559, #22993, #15498, #15606, #10686, #2843, #7232, #6634, #24948, #2911, #22675, #14879, #24487, #18290, #12984, #10045, #24883, #17937, #22405, #6125, #10296, #18422, #16012, #8226, #6157, #12989, #1212, #7800, #21001, #11650, #3166, #14024, #24098, #20274, #14437, #4427, #2558, #25393, #11024, #4056, #3670, #13443, #7669, #4156, #18381, #22043, #22141, #2633, #98, #9318, #7642, #15015, #260, #22248, #9418, #2179, #12166, #10199, #10764, #21654, #8135, #3873, #18081, #15181, #19764, #416, #3673, #11106, #17748, #23956, #9800, #2951, #11547, #3223, #8693, #25777, #24150, #2881, #730, #22643, #21498, #15392, #606, #1921, #7891, #6453, #17015, #257, #411, #9463, #24984, #14290, #24074, #23659, #25561, #18907, #5042, #18456, #17717, #11911, #24340, #21479, #9629, #6731, #14924, #8193, #19411, #12242, #18259, #17173, #13756, #9641, #2247, #10208, #25389, #24124, #5457, #24695, #7202, #6056, #3640, #24014, #23767, #16340, #22890, #25800, #19597, #20568, #10532, #13217, #23785, #19091, #21313, #5232, #726, #2669, #23323, #10105, #12759, #23401, #7573, #313, #24377, #2712, #19527, #8520, #14140, #6781, #1760, #14051, #11549, #14658, #7324, #5289, #4363, #14727, #21377, #14699, #8908, #12107, #13986, #19207, #25347, #4305, #11155, #14408, #19217, #15553, #18120, #11815, #3019, #6575, #8639, #7235, #507, #10715, #23457, #22600, #17011, #9973, #18945, #10566, #25744, #14490, #18739, #7890, #1868, #5081, #23748, #1107, #14013, #18228, #11471, #18996 ) ) ;
#24410 = CARTESIAN_POINT ( 'NONE',  ( 3.756430356249996105, -27.69062499938548072, 6.831223922626973533 ) ) ;
#24411 = CARTESIAN_POINT ( 'NONE',  ( -1.878215178124996498, 28.89062499938548711, 5.746835883940462963 ) ) ;
#24412 = CARTESIAN_POINT ( 'NONE',  ( -9.610428525061097460, -29.57785765677920509, -6.500000000000000000 ) ) ;
#24413 = DIRECTION ( 'NONE',  ( 1.000000000000000000, 0.000000000000000000, 0.000000000000000000 ) ) ;
#24414 = CARTESIAN_POINT ( 'NONE',  ( -5.706339097770933400, 38.63519838069944967, 7.645898033750358813 ) ) ;
#24415 = EDGE_CURVE ( 'NONE', #20933, #15851, #12608, .T. ) ;
#24416 = CARTESIAN_POINT ( 'NONE',  ( -3.959305739469038251E-15, -30.00000000000000355, 12.99999999999999289 ) ) ;
#24417 = DIRECTION ( 'NONE',  ( 0.000000000000000000, 0.000000000000000000, 1.000000000000000000 ) ) ;
#24418 = CARTESIAN_POINT ( 'NONE',  ( -26.00000000000000711, 0.000000000000000000, 20.00000000000000000 ) ) ;
#24419 = CARTESIAN_POINT ( 'NONE',  ( 17.29753586877772520, 19.95373324673703408, 12.25316411605951927 ) ) ;
#24420 = CARTESIAN_POINT ( 'NONE',  ( 19.19352969096333439, 22.02195681570944785, 5.535898384862237620 ) ) ;
#24421 = DIRECTION ( 'NONE',  ( 0.000000000000000000, -0.000000000000000000, 1.000000000000000000 ) ) ;
#24422 = DIRECTION ( 'NONE',  ( 0.000000000000000000, 0.000000000000000000, 1.000000000000000000 ) ) ;
#24423 = CARTESIAN_POINT ( 'NONE',  ( 3.756430356250003655, 26.04062499938548569, 8.999999999999992895 ) ) ;
#24425 = ORIENTED_EDGE ( 'NONE', *, *, #4982, .F. ) ;
#24424 = DIRECTION ( 'NONE',  ( 1.000000000000000000, 0.000000000000000000, 0.000000000000000000 ) ) ;
#24426 = LINE ( 'NONE', #16465, #15836 ) ;
#24427 = CARTESIAN_POINT ( 'NONE',  ( 19.64299713866565611, 18.12724761081355140, 12.99999999999999467 ) ) ;
#24428 = VERTEX_POINT ( 'NONE', #20416 ) ;
#24429 = CYLINDRICAL_SURFACE ( 'NONE', #8828, 4.000000000000000000 ) ;
#24430 = DIRECTION ( 'NONE',  ( -0.000000000000000000, -0.000000000000000000, 1.000000000000000000 ) ) ;
#24431 = CARTESIAN_POINT ( 'NONE',  ( 1.878215178124995832, -26.19062499938548427, 5.746835883940462963 ) ) ;
#24433 = VERTEX_POINT ( 'NONE', #16255 ) ;
#24432 = CYLINDRICAL_SURFACE ( 'NONE', #15850, 31.10000000000000142 ) ;
#24434 = CARTESIAN_POINT ( 'NONE',  ( -27.00874656207317059, -15.41874213889385459, 1.000000000000000000 ) ) ;
#24435 =( BOUNDED_CURVE ( )  B_SPLINE_CURVE ( 2, ( #23982, #20045, #2527, #20575, #4359, #18496, #12455, #24102, #10115 ),
 .UNSPECIFIED., .F., .F. ) 
 B_SPLINE_CURVE_WITH_KNOTS ( ( 3, 2, 2, 2, 3 ),
 ( 0.7249999999999999778, 0.7333333333333332815, 0.7500000000000000000, 0.7666666666666667185, 0.7750000000000000222 ),
 .UNSPECIFIED. ) 
 CURVE ( )  GEOMETRIC_REPRESENTATION_ITEM ( )  RATIONAL_B_SPLINE_CURVE ( ( 0.9330127018922194093, 0.9330127018922194093, 1.000000000000000000, 0.8660254037844387076, 1.000000000000000000, 0.8660254037844387076, 1.000000000000000000, 0.9330127018922194093, 0.9330127018922194093 ) ) 
 REPRESENTATION_ITEM ( '' )  );
#24436 = EDGE_CURVE ( 'NONE', #12308, #5761, #86, .T. ) ;
#24437 = ORIENTED_EDGE ( 'NONE', *, *, #19712, .F. ) ;
#24438 = CARTESIAN_POINT ( 'NONE',  ( -3.756430356250002323, -26.00312499938548427, 11.16877607737301226 ) ) ;
#24439 = ORIENTED_EDGE ( 'NONE', *, *, #24343, .T. ) ;
#24440 = ORIENTED_EDGE ( 'NONE', *, *, #8103, .T. ) ;
#24441 = LINE ( 'NONE', #10430, #3043 ) ;
#24442 = FACE_OUTER_BOUND ( 'NONE', #10653, .T. ) ;
#24443 = DIRECTION ( 'NONE',  ( 0.000000000000000000, 0.000000000000000000, 1.000000000000000000 ) ) ;
#24444 = CARTESIAN_POINT ( 'NONE',  ( -3.756430356249996994, -8.999999999999992895, 0.9281249993854829849 ) ) ;
#24445 = FILL_AREA_STYLE ('',( #11088 ) ) ;
#24446 = CYLINDRICAL_SURFACE ( 'NONE', #3437, 4.000000000000000000 ) ;
#24447 = CARTESIAN_POINT ( 'NONE',  ( 3.735045420075836212E-15, 25.70312499938548001, 4.662447845253954171 ) ) ;
#24448 = DIRECTION ( 'NONE',  ( -0.000000000000000000, -0.000000000000000000, 1.000000000000000000 ) ) ;
#24449 = CARTESIAN_POINT ( 'NONE',  ( 3.999999999999997335, -28.86250000000000071, 11.30940107675849404 ) ) ;
#24450 = CARTESIAN_POINT ( 'NONE',  ( 1.878215178125004048, 25.66562499938548569, 5.746835883940462963 ) ) ;
#24451 = CARTESIAN_POINT ( 'NONE',  ( -3.999999999999996447, -8.999999999999992895, 0.000000000000000000 ) ) ;
#24452 = DIRECTION ( 'NONE',  ( 0.000000000000000000, 0.000000000000000000, 1.000000000000000000 ) ) ;
#24453 = CARTESIAN_POINT ( 'NONE',  ( 3.834746474454188013E-15, 28.65624999877096712, 4.999999999999992006 ) ) ;
#24454 = CARTESIAN_POINT ( 'NONE',  ( 3.756430356249995661, -26.34062499938548285, 6.831223922626973533 ) ) ;
#24455 = DIRECTION ( 'NONE',  ( 1.000000000000000000, 0.000000000000000000, 0.000000000000000000 ) ) ;
#24456 = DIRECTION ( 'NONE',  ( 0.000000000000000000, 0.000000000000000000, 1.000000000000000000 ) ) ;
#24457 = CARTESIAN_POINT ( 'NONE',  ( 0.000000000000000000, 0.000000000000000000, -6.500000000000000000 ) ) ;
#24458 = CARTESIAN_POINT ( 'NONE',  ( 0.2646063747045178660, -30.00000000000000000, 4.999999999999992895 ) ) ;
#24459 = EDGE_CURVE ( 'NONE', #24369, #14282, #19282, .T. ) ;
#24460 = ORIENTED_EDGE ( 'NONE', *, *, #853, .F. ) ;
#24461 = AXIS2_PLACEMENT_3D ( 'NONE', #2885, #18592, #12711 ) ;
#24462 = CARTESIAN_POINT ( 'NONE',  ( 4.000000000000002665, 27.68124999877097281, 6.690598923241489970 ) ) ;
#24464 = ORIENTED_EDGE ( 'NONE', *, *, #25125, .T. ) ;
#24463 = DIRECTION ( 'NONE',  ( 0.000000000000000000, -0.000000000000000000, 1.000000000000000000 ) ) ;
#24465 = VERTEX_POINT ( 'NONE', #2388 ) ;
#24466 = ORIENTED_EDGE ( 'NONE', *, *, #23531, .T. ) ;
#24467 = ORIENTED_EDGE ( 'NONE', *, *, #1570, .T. ) ;
#24468 = ORIENTED_EDGE ( 'NONE', *, *, #197, .F. ) ;
#24469 = ORIENTED_EDGE ( 'NONE', *, *, #4088, .F. ) ;
#24470 = CARTESIAN_POINT ( 'NONE',  ( 3.756430356250003655, 25.14062499938548356, 8.999999999999992895 ) ) ;
#24471 = EDGE_CURVE ( 'NONE', #2042, #13481, #16397, .T. ) ;
#24472 = ORIENTED_EDGE ( 'NONE', *, *, #15099, .T. ) ;
#24473 = CARTESIAN_POINT ( 'NONE',  ( -13.24173596767339767, 28.14012133169338270, 1.000000000000000000 ) ) ;
#24474 = DIRECTION ( 'NONE',  ( 1.000000000000000000, 0.000000000000000000, 0.000000000000000000 ) ) ;
#24475 = CARTESIAN_POINT ( 'NONE',  ( -1.878215178124998497, -12.25316411605951927, 2.803124999385484539 ) ) ;
#24476 = CARTESIAN_POINT ( 'NONE',  ( -1.999999999999998224, -12.46410161513774639, 0.6937499987709692117 ) ) ;
#24477 = CARTESIAN_POINT ( 'NONE',  ( 20.43103032403801578, 17.77483294607857189, 5.746835883940462963 ) ) ;
#24478 = CARTESIAN_POINT ( 'NONE',  ( 0.000000000000000000, 0.000000000000000000, -6.500000000000000000 ) ) ;
#24479 = FACE_OUTER_BOUND ( 'NONE', #21235, .T. ) ;
#24480 = CARTESIAN_POINT ( 'NONE',  ( 1.878215178125000939, -12.25316411605952283, 2.765624999385481786 ) ) ;
#24481 = CARTESIAN_POINT ( 'NONE',  ( -3.999999999999996003, -6.690598923241487306, 4.237499999999998046 ) ) ;
#24482 = CARTESIAN_POINT ( 'NONE',  ( -3.756430356250003655, -25.19687499938548569, 8.999999999999992895 ) ) ;
#24483 = CARTESIAN_POINT ( 'NONE',  ( -1.878215178124995832, 28.44062499938548427, 5.746835883940462963 ) ) ;
#24484 = CARTESIAN_POINT ( 'NONE',  ( -3.756430356249996105, -6.831223922626973533, 2.240624999385484539 ) ) ;
#24485 = CARTESIAN_POINT ( 'NONE',  ( 4.000000000000001776, 27.60624999877096641, 11.30940107675849760 ) ) ;
#24486 = VERTEX_POINT ( 'NONE', #18343 ) ;
#24487 = ORIENTED_EDGE ( 'NONE', *, *, #24156, .T. ) ;
#24488 = CARTESIAN_POINT ( 'NONE',  ( -3.756430356249997882, 28.62812499938548783, 8.999999999999992895 ) ) ;
#24489 = EDGE_CURVE ( 'NONE', #5294, #21622, #14952, .T. ) ;
#24490 = VERTEX_POINT ( 'NONE', #3005 ) ;
#24491 = DIRECTION ( 'NONE',  ( 0.000000000000000000, 0.000000000000000000, 1.000000000000000000 ) ) ;
#24492 = ORIENTED_EDGE ( 'NONE', *, *, #2302, .F. ) ;
#24493 = CARTESIAN_POINT ( 'NONE',  ( 2.000000000000003997, -5.535898384862238508, 2.268749998770969167 ) ) ;
#24494 = ADVANCED_FACE ( 'NONE', ( #22390 ), #10976, .T. ) ;
#24495 = ORIENTED_EDGE ( 'NONE', *, *, #14830, .T. ) ;
#24496 = DIRECTION ( 'NONE',  ( 0.06279051952932236669, 0.9980267284282710039, 0.000000000000000000 ) ) ;
#24497 = DIRECTION ( 'NONE',  ( -0.6845471059286901694, -0.7289686274214101092, 0.000000000000000000 ) ) ;
#24498 = ORIENTED_EDGE ( 'NONE', *, *, #18335, .F. ) ;
#24499 = EDGE_CURVE ( 'NONE', #7895, #24428, #15035, .T. ) ;
#24500 = DIRECTION ( 'NONE',  ( 0.3090169943749591086, 0.9510565162951497564, 0.000000000000000000 ) ) ;
#24501 = CARTESIAN_POINT ( 'NONE',  ( -3.756430356249996994, 28.96562499938548285, 8.999999999999992895 ) ) ;
#24502 = DIRECTION ( 'NONE',  ( 0.000000000000000000, 0.000000000000000000, 1.000000000000000000 ) ) ;
#24503 = DIRECTION ( 'NONE',  ( -1.000000000000000000, 0.000000000000000000, 0.000000000000000000 ) ) ;
#24504 = CARTESIAN_POINT ( 'NONE',  ( 4.648177544792955347E-16, 26.68750000000000711, 12.99999999999999289 ) ) ;
#24505 = FACE_OUTER_BOUND ( 'NONE', #18276, .T. ) ;
#24506 = CARTESIAN_POINT ( 'NONE',  ( -1.878215178124998497, 27.24062499938548498, 12.25316411605951927 ) ) ;
#24507 = CARTESIAN_POINT ( 'NONE',  ( 18.09530447186750024, 18.09530447186743629, 13.33755215474603162 ) ) ;
#24508 = CYLINDRICAL_SURFACE ( 'NONE', #23333, 0.5000000000000004441 ) ;
#24509 = CARTESIAN_POINT ( 'NONE',  ( -1.999999999999993117, 25.99374999877097281, 5.535898384862237620 ) ) ;
#24510 = DIRECTION ( 'NONE',  ( 1.000000000000000000, 0.000000000000000000, 0.000000000000000000 ) ) ;
#24511 = CARTESIAN_POINT ( 'NONE',  ( -3.756430356250003211, -26.52812499938548285, 6.831223922626973533 ) ) ;
#24512 = CARTESIAN_POINT ( 'NONE',  ( 4.000000000000003553, 25.39374999877097494, 8.999999999999992895 ) ) ;
#24513 = VERTEX_POINT ( 'NONE', #918 ) ;
#24514 = CARTESIAN_POINT ( 'NONE',  ( -1.878215178124995832, 26.30312499938548498, 5.746835883940462963 ) ) ;
#24515 = CARTESIAN_POINT ( 'NONE',  ( 3.999999999999996003, -29.23750000000000071, 6.690598923241487306 ) ) ;
#24517 = EDGE_LOOP ( 'NONE', ( #17809, #19087, #11761, #5669 ) ) ;
#24516 = CARTESIAN_POINT ( 'NONE',  ( -1.878215178124996498, 27.65312499938548996, 5.746835883940462963 ) ) ;
#24518 = ORIENTED_EDGE ( 'NONE', *, *, #8746, .F. ) ;
#24519 = CARTESIAN_POINT ( 'NONE',  ( 0.000000000000000000, 0.000000000000000000, 0.000000000000000000 ) ) ;
#24520 = CARTESIAN_POINT ( 'NONE',  ( 2.000000000000003997, 26.36874999877096926, 5.535898384862238508 ) ) ;
#24521 = ORIENTED_EDGE ( 'NONE', *, *, #24665, .T. ) ;
#24522 = EDGE_CURVE ( 'NONE', #16527, #15624, #18221, .T. ) ;
#24523 = CARTESIAN_POINT ( 'NONE',  ( -3.756430356250003655, -26.15312499938548640, 8.999999999999992895 ) ) ;
#24524 = CARTESIAN_POINT ( 'NONE',  ( 0.000000000000000000, 28.62812499938549138, 13.33755215474602984 ) ) ;
#24525 = DIRECTION ( 'NONE',  ( 1.000000000000000000, 0.000000000000000000, 0.000000000000000000 ) ) ;
#24526 = EDGE_CURVE ( 'NONE', #1309, #5799, #8855, .T. ) ;
#24527 = DIRECTION ( 'NONE',  ( 1.000000000000000000, 0.000000000000000000, 0.000000000000000000 ) ) ;
#24528 = DIRECTION ( 'NONE',  ( 0.000000000000000000, 0.000000000000000000, 1.000000000000000000 ) ) ;
#24529 = CARTESIAN_POINT ( 'NONE',  ( 16.62584819264874270, 22.28270244214105134, 11.30940107675849404 ) ) ;
#24530 = LINE ( 'NONE', #18399, #23450 ) ;
#24531 = CIRCLE ( 'NONE', #14117, 0.5000000000000004441 ) ;
#24532 = CARTESIAN_POINT ( 'NONE',  ( 3.756430356250003211, 25.17812499938548498, 6.831223922626973533 ) ) ;
#24533 = LINE ( 'NONE', #10796, #8707 ) ;
#24534 = CARTESIAN_POINT ( 'NONE',  ( 22.34249210749660364, 17.03009735157778337, 8.999999999999992895 ) ) ;
#24535 = CARTESIAN_POINT ( 'NONE',  ( 22.03079565047434585, 16.37394140098190221, 11.30940107675849760 ) ) ;
#24536 = CARTESIAN_POINT ( 'NONE',  ( 4.000000000000003553, 29.69687499938548569, 8.999999999999992895 ) ) ;
#24537 = DIRECTION ( 'NONE',  ( -0.000000000000000000, 0.000000000000000000, 1.000000000000000000 ) ) ;
#24538 = CARTESIAN_POINT ( 'NONE',  ( -1.878215178124995832, 25.74062499938548498, 5.746835883940462963 ) ) ;
#24540 = ORIENTED_EDGE ( 'NONE', *, *, #9570, .F. ) ;
#24539 = DIRECTION ( 'NONE',  ( -0.6374239897486919659, -0.7705132427757873659, 0.000000000000000000 ) ) ;
#24541 = FACE_OUTER_BOUND ( 'NONE', #7510, .T. ) ;
#24542 = DIRECTION ( 'NONE',  ( -1.000000000000000000, 0.000000000000000000, 0.000000000000000000 ) ) ;
#24543 = VERTEX_POINT ( 'NONE', #9017 ) ;
#24544 = CARTESIAN_POINT ( 'NONE',  ( -6.317933499822993682, 30.45149776762736593, 1.000000000000000000 ) ) ;
#24545 = CARTESIAN_POINT ( 'NONE',  ( 4.000000000000003553, 26.78124999877097068, 6.690598923241489970 ) ) ;
#24546 = CARTESIAN_POINT ( 'NONE',  ( 3.756430356249995661, -27.12812499938548427, 6.831223922626973533 ) ) ;
#24548 = ORIENTED_EDGE ( 'NONE', *, *, #10988, .T. ) ;
#24547 = CARTESIAN_POINT ( 'NONE',  ( 0.000000000000000000, 0.000000000000000000, -6.500000000000000000 ) ) ;
#24549 = DIRECTION ( 'NONE',  ( -0.000000000000000000, -0.000000000000000000, -1.000000000000000000 ) ) ;
#24550 = ORIENTED_EDGE ( 'NONE', *, *, #11543, .F. ) ;
#24551 = EDGE_CURVE ( 'NONE', #12308, #23924, #15543, .T. ) ;
#24552 = CARTESIAN_POINT ( 'NONE',  ( 3.756430356249996994, -25.36562499938548498, 8.999999999999992895 ) ) ;
#24553 = VERTEX_POINT ( 'NONE', #6175 ) ;
#24554 = ORIENTED_EDGE ( 'NONE', *, *, #23753, .F. ) ;
#24555 = DIRECTION ( 'NONE',  ( 1.000000000000000000, -0.000000000000000000, 0.000000000000000000 ) ) ;
#24556 = CARTESIAN_POINT ( 'NONE',  ( 1.878215178124999829, 25.62812499938549138, 12.25316411605952283 ) ) ;
#24557 = EDGE_CURVE ( 'NONE', #14822, #10843, #20285, .T. ) ;
#24558 = CARTESIAN_POINT ( 'NONE',  ( -1.952785157361201618, 31.03863125411927371, -6.500000000000000000 ) ) ;
#24559 = CIRCLE ( 'NONE', #13295, 26.00000000000000711 ) ;
#24560 = CARTESIAN_POINT ( 'NONE',  ( -3.756430356249995661, -6.831223922626973533, 2.240624999385484539 ) ) ;
#24561 = CARTESIAN_POINT ( 'NONE',  ( -10.94867358849309547, 28.91604871112477326, 1.000000000000000000 ) ) ;
#24562 = CARTESIAN_POINT ( 'NONE',  ( -3.756430356249997882, 26.30312499938548498, 11.16877607737301226 ) ) ;
#24563 = EDGE_CURVE ( 'NONE', #24543, #10325, #22641, .T. ) ;
#24564 = CARTESIAN_POINT ( 'NONE',  ( -30.78811501957140706, 4.393401135981310546, 1.000000000000000000 ) ) ;
#24565 = CARTESIAN_POINT ( 'NONE',  ( 0.000000000000000000, 0.000000000000000000, 1.000000000000000000 ) ) ;
#24566 = UNCERTAINTY_MEASURE_WITH_UNIT (LENGTH_MEASURE( 1.000000000000000082E-05 ), #569, 'distance_accuracy_value', 'NONE');
#24567 = CARTESIAN_POINT ( 'NONE',  ( 3.756430356250003211, 29.22812499938548569, 6.831223922626973533 ) ) ;
#24568 = CARTESIAN_POINT ( 'NONE',  ( 3.897863563849872204, 30.85476721088026508, -6.500000000000000000 ) ) ;
#24569 = DIRECTION ( 'NONE',  ( 0.000000000000000000, 0.000000000000000000, 1.000000000000000000 ) ) ;
#24570 = CARTESIAN_POINT ( 'NONE',  ( 19.82550637751787548, 19.82550637751778666, 12.99999999999999289 ) ) ;
#24571 = CARTESIAN_POINT ( 'NONE',  ( -3.735045420075836212E-15, -26.26562499938548356, 4.662447845253954171 ) ) ;
#24572 = DIRECTION ( 'NONE',  ( 0.000000000000000000, -0.000000000000000000, 1.000000000000000000 ) ) ;
#24573 = VECTOR ( 'NONE', #13205, 1000.000000000000000 ) ;
#24574 = CARTESIAN_POINT ( 'NONE',  ( -18.28012134629613783, -25.16042852506070560, -6.500000000000000000 ) ) ;
#24575 = LINE ( 'NONE', #8516, #10536 ) ;
#24577 = ORIENTED_EDGE ( 'NONE', *, *, #14336, .F. ) ;
#24576 = AXIS2_PLACEMENT_3D ( 'NONE', #4285, #18402, #20098 ) ;
#24578 = CARTESIAN_POINT ( 'NONE',  ( 0.000000000000000000, 0.000000000000000000, -6.500000000000000000 ) ) ;
#24580 = VERTEX_POINT ( 'NONE', #21301 ) ;
#24579 = CYLINDRICAL_SURFACE ( 'NONE', #20402, 4.000000000000000000 ) ;
#24581 = CIRCLE ( 'NONE', #16659, 3.000000000000000444 ) ;
#24582 = ORIENTED_EDGE ( 'NONE', *, *, #23192, .T. ) ;
#24584 = ORIENTED_EDGE ( 'NONE', *, *, #23874, .F. ) ;
#24583 = VECTOR ( 'NONE', #4249, 1000.000000000000000 ) ;
#24585 = ORIENTED_EDGE ( 'NONE', *, *, #5772, .F. ) ;
#24586 = ORIENTED_EDGE ( 'NONE', *, *, #10394, .T. ) ;
#24587 = EDGE_CURVE ( 'NONE', #6155, #5488, #1297, .T. ) ;
#24588 = DIRECTION ( 'NONE',  ( 0.000000000000000000, 0.000000000000000000, 1.000000000000000000 ) ) ;
#24589 = ORIENTED_EDGE ( 'NONE', *, *, #16990, .T. ) ;
#24590 = DIRECTION ( 'NONE',  ( 0.000000000000000000, 0.000000000000000000, 1.000000000000000000 ) ) ;
#24591 = CARTESIAN_POINT ( 'NONE',  ( -1.878215178124995832, 29.00312499938548427, 5.746835883940462963 ) ) ;
#24592 = EDGE_CURVE ( 'NONE', #476, #5606, #22968, .T. ) ;
#24593 = VECTOR ( 'NONE', #788, 1000.000000000000000 ) ;
#24594 = CARTESIAN_POINT ( 'NONE',  ( 2.672651547586948120E-15, -13.33755215474602984, 2.390624999385484450 ) ) ;
#24595 = CIRCLE ( 'NONE', #19993, 0.5000000000000002220 ) ;
#24596 = PLANE ( 'NONE',  #24212 ) ;
#24597 = FACE_OUTER_BOUND ( 'NONE', #4580, .T. ) ;
#24598 = DIRECTION ( 'NONE',  ( 0.000000000000000000, 0.000000000000000000, 1.000000000000000000 ) ) ;
#24599 = VECTOR ( 'NONE', #2420, 1000.000000000000000 ) ;
#24600 = EDGE_CURVE ( 'NONE', #12001, #1533, #13728, .T. ) ;
#24601 = CYLINDRICAL_SURFACE ( 'NONE', #10037, 0.5000000000000004441 ) ;
#24602 = AXIS2_PLACEMENT_3D ( 'NONE', #24574, #12816, #12552 ) ;
#24603 = CARTESIAN_POINT ( 'NONE',  ( -1.878215178124995832, -5.746835883940462963, 2.540624999385482141 ) ) ;
#24604 = CARTESIAN_POINT ( 'NONE',  ( -29.57785765677936851, -9.610428525060582317, -6.500000000000000000 ) ) ;
#24605 = CARTESIAN_POINT ( 'NONE',  ( -18.28012134629558716, 25.16042852506110705, -6.500000000000000000 ) ) ;
#24606 = DIRECTION ( 'NONE',  ( -0.000000000000000000, -0.000000000000000000, 1.000000000000000000 ) ) ;
#24607 = DIRECTION ( 'NONE',  ( 1.000000000000000000, 0.000000000000000000, 0.000000000000000000 ) ) ;
#24608 = CARTESIAN_POINT ( 'NONE',  ( 3.756430356250003211, -6.831223922626973533, 1.190624999385485383 ) ) ;
#24609 = CARTESIAN_POINT ( 'NONE',  ( 1.071796769724494558, 25.48615380933863150, 4.999999999999992006 ) ) ;
#24610 = FACE_OUTER_BOUND ( 'NONE', #11260, .T. ) ;
#24611 = ORIENTED_EDGE ( 'NONE', *, *, #3089, .T. ) ;
#24612 = ORIENTED_EDGE ( 'NONE', *, *, #20281, .F. ) ;
#24613 = CARTESIAN_POINT ( 'NONE',  ( 3.756430356250003211, 28.85312499938548569, 8.999999999999992895 ) ) ;
#24614 = VECTOR ( 'NONE', #8466, 1000.000000000000000 ) ;
#24615 = EDGE_LOOP ( 'NONE', ( #18049, #3529, #981, #797, #7680, #18319, #2425, #8187, #18320, #11154, #14073, #10140, #21723, #10461, #22492, #8770 ) ) ;
#24616 = ORIENTED_EDGE ( 'NONE', *, *, #25507, .T. ) ;
#24617 = DIRECTION ( 'NONE',  ( -0.000000000000000000, 1.000000000000000000, -0.000000000000000000 ) ) ;
#24618 = ORIENTED_EDGE ( 'NONE', *, *, #20649, .T. ) ;
#24619 = CARTESIAN_POINT ( 'NONE',  ( 0.000000000000000000, 0.000000000000000000, -6.500000000000000000 ) ) ;
#24620 = VECTOR ( 'NONE', #22022, 1000.000000000000000 ) ;
#24621 = AXIS2_PLACEMENT_3D ( 'NONE', #7501, #14045, #1889 ) ;
#24622 = EDGE_LOOP ( 'NONE', ( #3845, #24759, #6962, #18995 ) ) ;
#24623 = DIRECTION ( 'NONE',  ( 1.000000000000000000, 0.000000000000000000, 0.000000000000000000 ) ) ;
#24624 = CARTESIAN_POINT ( 'NONE',  ( 3.735045420075836212E-15, 29.30312499938548498, 4.662447845253954171 ) ) ;
#24625 = CARTESIAN_POINT ( 'NONE',  ( -3.834746474454188013E-15, -27.36250000000000426, 4.999999999999992006 ) ) ;
#24626 = EDGE_CURVE ( 'NONE', #19250, #10990, #4255, .T. ) ;
#24627 = CYLINDRICAL_SURFACE ( 'NONE', #18853, 4.000000000000000000 ) ;
#24628 = FACE_OUTER_BOUND ( 'NONE', #4164, .T. ) ;
#24629 = CARTESIAN_POINT ( 'NONE',  ( 19.20899765223631306, 19.20899765223624200, 4.662447845253954171 ) ) ;
#24630 =( GEOMETRIC_REPRESENTATION_CONTEXT ( 3 ) GLOBAL_UNCERTAINTY_ASSIGNED_CONTEXT ( ( #24566 ) ) GLOBAL_UNIT_ASSIGNED_CONTEXT ( ( #569, #22025, #21776 ) ) REPRESENTATION_CONTEXT ( 'NONE', 'WORKASPACE' ) );
#24631 = EDGE_CURVE ( 'NONE', #3398, #4306, #931, .T. ) ;
#24632 = CARTESIAN_POINT ( 'NONE',  ( 3.756430356250002323, 27.80312499938548143, 11.16877607737301226 ) ) ;
#24633 = VECTOR ( 'NONE', #16056, 1000.000000000000000 ) ;
#24634 = DIRECTION ( 'NONE',  ( -1.000000000000000000, 0.000000000000000000, 0.000000000000000000 ) ) ;
#24635 = CARTESIAN_POINT ( 'NONE',  ( 3.959305671612554781E-15, 35.50000000000000711, 12.99999999999999289 ) ) ;
#24636 = CARTESIAN_POINT ( 'NONE',  ( 4.000000000000003553, -8.999999999999992895, 2.249999999999998668 ) ) ;
#24637 = ADVANCED_FACE ( 'NONE', ( #11743, #3516, #25613 ), #25480, .T. ) ;
#24638 = CARTESIAN_POINT ( 'NONE',  ( -4.000000000000000000, 26.06874999877097210, 8.999999999999992895 ) ) ;
#24639 = CARTESIAN_POINT ( 'NONE',  ( 3.756430356250004987, 29.75312499938549138, 8.999999999999992895 ) ) ;
#24640 = CARTESIAN_POINT ( 'NONE',  ( -3.756430356250003211, -27.42812499938548143, 6.831223922626973533 ) ) ;
#24641 = CARTESIAN_POINT ( 'NONE',  ( 2.620986760973688460E-15, -13.61880215351699874, 0.3375000000000007438 ) ) ;
#24642 = CIRCLE ( 'NONE', #14199, 0.5000000000000003331 ) ;
#24643 = ORIENTED_EDGE ( 'NONE', *, *, #2543, .T. ) ;
#24644 = B_SPLINE_CURVE_WITH_KNOTS ( 'NONE', 3,
 ( #11354, #15286, #5603, #15793, #3630, #17262, #15673, #9398, #13581, #21549 ),
 .UNSPECIFIED., .F., .F.,
 ( 4, 2, 2, 2, 4 ),
 ( 0.01251976117704806969, 0.01338929815772730951, 0.01425883513840654759, 0.01512837211908578741, 0.01599790909976502723 ),
 .UNSPECIFIED. ) ;
#24645 = CARTESIAN_POINT ( 'NONE',  ( -1.878215178124998497, 25.55312499938548854, 12.25316411605951927 ) ) ;
#24646 = CARTESIAN_POINT ( 'NONE',  ( -16.66421332384646448, 26.25859848311288403, 1.000000000000000000 ) ) ;
#24648 = ORIENTED_EDGE ( 'NONE', *, *, #8373, .T. ) ;
#24647 = CARTESIAN_POINT ( 'NONE',  ( -3.756430356249995661, -6.831223922626973533, 0.3281249993854827851 ) ) ;
#24649 = ORIENTED_EDGE ( 'NONE', *, *, #18931, .T. ) ;
#24650 = CARTESIAN_POINT ( 'NONE',  ( 1.071796769724488563, -29.31115380933863790, 12.99999999999999289 ) ) ;
#24651 =( BOUNDED_CURVE ( )  B_SPLINE_CURVE ( 2, ( #13590, #1689, #15802, #9663, #2070, #22064, #24154 ),
 .UNSPECIFIED., .F., .T. ) 
 B_SPLINE_CURVE_WITH_KNOTS ( ( 3, 2, 2, 3 ),
 ( 0.4999999999999997780, 0.5166666666666664964, 0.5333333333333329929, 0.5499999999999997113 ),
 .UNSPECIFIED. ) 
 CURVE ( )  GEOMETRIC_REPRESENTATION_ITEM ( )  RATIONAL_B_SPLINE_CURVE ( ( 1.000000000000001776, 0.8660254037844369313, 1.000000000000000000, 0.8660254037844387076, 1.000000000000000000, 0.8660254037844413721, 0.9999999999999973355 ) ) 
 REPRESENTATION_ITEM ( '' )  );
#24652 = VECTOR ( 'NONE', #4565, 1000.000000000000000 ) ;
#24653 = VECTOR ( 'NONE', #5997, 1000.000000000000000 ) ;
#24654 = ORIENTED_EDGE ( 'NONE', *, *, #5687, .T. ) ;
#24655 = EDGE_CURVE ( 'NONE', #15624, #21567, #3827, .T. ) ;
#24656 = CLOSED_SHELL ( 'NONE', ( #2399, #17222, #9644, #7705, #24018, #5726, #13559, #21700, #9631, #16205, #2896, #24674, #12986, #23634, #270, #17544, #8535, #1958, #6101, #2845, #1005, #6271, #22346, #11633, #25516, #19665, #17807, #23157, #16136, #1326, #1874, #12057 ) ) ;
#24657 = CARTESIAN_POINT ( 'NONE',  ( -1.878215178125000939, -26.97812499938548569, 12.25316411605952283 ) ) ;
#24658 = CARTESIAN_POINT ( 'NONE',  ( -27.10000000000000497, 0.6000000000000000888, 19.59999999999999787 ) ) ;
#24659 = CARTESIAN_POINT ( 'NONE',  ( 3.756430356250003211, 25.59062499938548285, 8.999999999999992895 ) ) ;
#24660 = AXIS2_PLACEMENT_3D ( 'NONE', #3961, #12319, #12440 ) ;
#24661 = CARTESIAN_POINT ( 'NONE',  ( -1.878215178124998497, -12.25316411605951927, 4.490624999385482319 ) ) ;
#24662 = CARTESIAN_POINT ( 'NONE',  ( 3.756430356250002323, 26.52812499938548640, 6.831223922626973533 ) ) ;
#24663 = VECTOR ( 'NONE', #7542, 1000.000000000000000 ) ;
#24664 = FACE_OUTER_BOUND ( 'NONE', #24915, .T. ) ;
#24665 = EDGE_CURVE ( 'NONE', #4649, #23534, #10431, .T. ) ;
#24666 = DIRECTION ( 'NONE',  ( 0.000000000000000000, 0.000000000000000000, -1.000000000000000000 ) ) ;
#24667 = VECTOR ( 'NONE', #15799, 1000.000000000000000 ) ;
#24668 = CIRCLE ( 'NONE', #3369, 6.000000000000000000 ) ;
#24669 = DIRECTION ( 'NONE',  ( -0.000000000000000000, -1.000000000000000000, -0.000000000000000000 ) ) ;
#24670 = CARTESIAN_POINT ( 'NONE',  ( 19.34820930021694352, 19.34820930021687246, 4.999999999999992006 ) ) ;
#24671 = CARTESIAN_POINT ( 'NONE',  ( 1.999999999999998224, -28.39374999877096784, 12.46410161513774639 ) ) ;
#24672 = CARTESIAN_POINT ( 'NONE',  ( 21.36138144860026600, 16.04898669268145639, 11.16877607737301226 ) ) ;
#24673 = CARTESIAN_POINT ( 'NONE',  ( 16.74068927859332234, 19.39688665655263122, 12.25316411605951927 ) ) ;
#24674 = ADVANCED_FACE ( 'NONE', ( #7186 ), #15174, .T. ) ;
#24675 = AXIS2_PLACEMENT_3D ( 'NONE', #14076, #96, #12488 ) ;
#24676 = CARTESIAN_POINT ( 'NONE',  ( 1.626862140677534194E-14, 27.58750000000000213, 12.99999999999999289 ) ) ;
#24677 = CARTESIAN_POINT ( 'NONE',  ( -3.959305671612554781E-15, -30.00000000000000355, 12.99999999999999289 ) ) ;
#24678 = CARTESIAN_POINT ( 'NONE',  ( 2.672651547586948120E-15, 27.27812499938548285, 13.33755215474602984 ) ) ;
#24680 = EDGE_CURVE ( 'NONE', #17275, #16526, #21435, .T. ) ;
#24679 = AXIS2_PLACEMENT_3D ( 'NONE', #18156, #9778, #233 ) ;
#24682 = ORIENTED_EDGE ( 'NONE', *, *, #7481, .T. ) ;
#24681 = CARTESIAN_POINT ( 'NONE',  ( -26.50000000000000355, -0.5000000000000000000, 19.50000000000000000 ) ) ;
#24683 = CARTESIAN_POINT ( 'NONE',  ( 3.469446951953614189E-15, 46.00000000000000000, 8.999999999999992895 ) ) ;
#24684 = CARTESIAN_POINT ( 'NONE',  ( -26.25859848311282363, -16.66421332384654974, 1.000000000000000000 ) ) ;
#24685 = ORIENTED_EDGE ( 'NONE', *, *, #14043, .F. ) ;
#24686 = DIRECTION ( 'NONE',  ( 0.000000000000000000, -0.000000000000000000, 1.000000000000000000 ) ) ;
#24687 = CARTESIAN_POINT ( 'NONE',  ( -3.999999999999997335, 28.80624999877096926, 11.30940107675849404 ) ) ;
#24688 = CARTESIAN_POINT ( 'NONE',  ( -1.878215178125000939, -25.96562499938548285, 12.25316411605952283 ) ) ;
#24690 = ORIENTED_EDGE ( 'NONE', *, *, #15086, .F. ) ;
#24689 = CARTESIAN_POINT ( 'NONE',  ( 23.96296185032708337, 19.82388608118420237, 1.000000000000000000 ) ) ;
#24691 = FACE_OUTER_BOUND ( 'NONE', #23433, .T. ) ;
#24692 = CIRCLE ( 'NONE', #5479, 0.4999999999999991673 ) ;
#24693 = ORIENTED_EDGE ( 'NONE', *, *, #604, .T. ) ;
#24694 = CARTESIAN_POINT ( 'NONE',  ( -3.735045420075836212E-15, -25.70312499938548001, 4.662447845253954171 ) ) ;
#24695 = ORIENTED_EDGE ( 'NONE', *, *, #6590, .T. ) ;
#24696 = VERTEX_POINT ( 'NONE', #19201 ) ;
#24697 = FACE_OUTER_BOUND ( 'NONE', #24622, .T. ) ;
#24698 = CIRCLE ( 'NONE', #4640, 0.5000000000000004441 ) ;
#24699 = CARTESIAN_POINT ( 'NONE',  ( 1.878215178125005158, 27.12812499938548783, 5.746835883940462963 ) ) ;
#24700 = CIRCLE ( 'NONE', #12578, 4.000000000000000000 ) ;
#24701 = CARTESIAN_POINT ( 'NONE',  ( 2.000000000000003997, 27.77500000000000213, 5.535898384862238508 ) ) ;
#24702 = CIRCLE ( 'NONE', #13003, 0.5000000000000004441 ) ;
#24703 = CARTESIAN_POINT ( 'NONE',  ( 1.878215178125004048, -5.746835883940462963, 2.128124999385486049 ) ) ;
#24704 = DIRECTION ( 'NONE',  ( 1.000000000000000000, 0.000000000000000000, 0.000000000000000000 ) ) ;
#24705 = CARTESIAN_POINT ( 'NONE',  ( 3.756430356250002323, 28.70312499938548356, 11.16877607737301226 ) ) ;
#24706 = DIRECTION ( 'NONE',  ( 8.881784197001254296E-16, 0.000000000000000000, 1.000000000000000000 ) ) ;
#24707 = DIRECTION ( 'NONE',  ( 0.000000000000000000, 0.000000000000000000, 1.000000000000000000 ) ) ;
#24708 = CARTESIAN_POINT ( 'NONE',  ( 3.735045420075836212E-15, 28.40312499938548640, 4.662447845253954171 ) ) ;
#24709 = CARTESIAN_POINT ( 'NONE',  ( 19.62663259444009611, 19.62663259444001085, 4.999999999999992006 ) ) ;
#24710 = CARTESIAN_POINT ( 'NONE',  ( 23.26836714124207361, 18.93629030671969460, 11.57226653943513028 ) ) ;
#24711 = DIRECTION ( 'NONE',  ( 1.000000000000000000, 0.000000000000000000, 0.000000000000000000 ) ) ;
#24712 = EDGE_CURVE ( 'NONE', #20366, #5872, #1552, .T. ) ;
#24713 = CARTESIAN_POINT ( 'NONE',  ( 3.756430356249997882, -27.76562499938549067, 11.16877607737301226 ) ) ;
#24714 = VECTOR ( 'NONE', #25579, 1000.000000000000000 ) ;
#24715 = CARTESIAN_POINT ( 'NONE',  ( 0.000000000000000000, 0.000000000000000000, 1.000000000000000000 ) ) ;
#24716 = EDGE_CURVE ( 'NONE', #24827, #15870, #19688, .T. ) ;
#24717 = AXIS2_PLACEMENT_3D ( 'NONE', #15453, #25134, #24996 ) ;
#24718 = FACE_OUTER_BOUND ( 'NONE', #3111, .T. ) ;
#24719 = LINE ( 'NONE', #4721, #6226 ) ;
#24720 = PLANE ( 'NONE',  #25167 ) ;
#24721 = ORIENTED_EDGE ( 'NONE', *, *, #14533, .T. ) ;
#24722 = CYLINDRICAL_SURFACE ( 'NONE', #15022, 31.10000000000000142 ) ;
#24724 = EDGE_LOOP ( 'NONE', ( #8087, #19975, #6965, #19502 ) ) ;
#24723 = DIRECTION ( 'NONE',  ( 0.000000000000000000, 0.000000000000000000, 1.000000000000000000 ) ) ;
#24725 = EDGE_CURVE ( 'NONE', #5826, #23600, #8430, .T. ) ;
#24726 = CIRCLE ( 'NONE', #5919, 0.5000000000000003331 ) ;
#24727 = ORIENTED_EDGE ( 'NONE', *, *, #300, .T. ) ;
#24728 = ORIENTED_EDGE ( 'NONE', *, *, #9136, .T. ) ;
#24729 = EDGE_LOOP ( 'NONE', ( #25145, #11500, #4881, #2781 ) ) ;
#24730 = VERTEX_POINT ( 'NONE', #12383 ) ;
#24731 = DIRECTION ( 'NONE',  ( 0.000000000000000000, 0.000000000000000000, -1.000000000000000000 ) ) ;
#24732 = CIRCLE ( 'NONE', #12199, 31.10000000000000142 ) ;
#24733 = ORIENTED_EDGE ( 'NONE', *, *, #23084, .F. ) ;
#24734 = DIRECTION ( 'NONE',  ( 0.000000000000000000, 0.000000000000000000, 1.000000000000000000 ) ) ;
#24735 = CARTESIAN_POINT ( 'NONE',  ( -3.756430356249996105, 29.49062499938548498, 6.831223922626973533 ) ) ;
#24736 = AXIS2_PLACEMENT_3D ( 'NONE', #1891, #17837, #25806 ) ;
#24737 = AXIS2_PLACEMENT_3D ( 'NONE', #23142, #19076, #3243 ) ;
#24738 = CARTESIAN_POINT ( 'NONE',  ( 2.672651547586948120E-15, -13.33755215474602984, 0.4781249993854826963 ) ) ;
#24739 = LINE ( 'NONE', #20681, #4176 ) ;
#24740 = VECTOR ( 'NONE', #16687, 1000.000000000000000 ) ;
#24741 = CARTESIAN_POINT ( 'NONE',  ( 3.959305671612554781E-15, 35.50000000000000711, 12.99999999999999289 ) ) ;
#24742 = DIRECTION ( 'NONE',  ( 0.000000000000000000, 0.000000000000000000, 1.000000000000000000 ) ) ;
#24743 = CARTESIAN_POINT ( 'NONE',  ( 6.741346781237209207, -25.16843286583315731, 20.00001199999999812 ) ) ;
#24744 = CARTESIAN_POINT ( 'NONE',  ( -3.756430356249997882, -11.16877607737301226, 4.453124999385482674 ) ) ;
#24745 = CARTESIAN_POINT ( 'NONE',  ( -26.50000000000000355, 0.5000000000000000000, 19.00000000000000000 ) ) ;
#24746 = CARTESIAN_POINT ( 'NONE',  ( 4.000000000000003553, -8.999999999999992895, 3.599999999999999201 ) ) ;
#24747 = DIRECTION ( 'NONE',  ( -0.000000000000000000, -1.000000000000000000, -0.000000000000000000 ) ) ;
#24748 = EDGE_CURVE ( 'NONE', #15602, #2722, #18162, .T. ) ;
#24749 = DIRECTION ( 'NONE',  ( 0.000000000000000000, 0.000000000000000000, -1.000000000000000000 ) ) ;
#24750 = CARTESIAN_POINT ( 'NONE',  ( 1.878215178125004048, -5.746835883940462963, 2.128124999385486049 ) ) ;
#24751 = ADVANCED_FACE ( 'NONE', ( #7950 ), #22327, .T. ) ;
#24752 = CARTESIAN_POINT ( 'NONE',  ( 1.071796769724494558, 27.73615380933863861, 4.999999999999992895 ) ) ;
#24753 = AXIS2_PLACEMENT_3D ( 'NONE', #18293, #20509, #2850 ) ;
#24754 = DIRECTION ( 'NONE',  ( 0.000000000000000000, 0.000000000000000000, 1.000000000000000000 ) ) ;
#24755 = EDGE_LOOP ( 'NONE', ( #15538, #8138, #18083, #16978 ) ) ;
#24756 = ORIENTED_EDGE ( 'NONE', *, *, #4093, .T. ) ;
#24757 = CARTESIAN_POINT ( 'NONE',  ( 3.756430356250004543, 27.01562499938549067, 11.16877607737301226 ) ) ;
#24758 = CIRCLE ( 'NONE', #23100, 0.4999999999999998890 ) ;
#24759 = ORIENTED_EDGE ( 'NONE', *, *, #13059, .T. ) ;
#24760 = LINE ( 'NONE', #25273, #25831 ) ;
#24761 = VERTEX_POINT ( 'NONE', #10284 ) ;
#24762 = CARTESIAN_POINT ( 'NONE',  ( 1.878215178124998497, -26.45312499938548711, 12.25316411605951927 ) ) ;
#24763 = VERTEX_POINT ( 'NONE', #12126 ) ;
#24764 = CARTESIAN_POINT ( 'NONE',  ( -3.469446951953614189E-15, -25.00000000000000000, 4.999999999999992006 ) ) ;
#24765 = EDGE_CURVE ( 'NONE', #933, #23953, #12280, .T. ) ;
#24766 = ORIENTED_EDGE ( 'NONE', *, *, #11921, .F. ) ;
#24767 = DIRECTION ( 'NONE',  ( -0.9980267284282710039, 0.06279051952932233893, 0.000000000000000000 ) ) ;
#24768 = CARTESIAN_POINT ( 'NONE',  ( 3.752267015613588906E-15, 26.01249999999999929, 4.381197846482986158 ) ) ;
#24769 = CARTESIAN_POINT ( 'NONE',  ( -3.999999999999997335, 28.35624999877096997, 11.30940107675849404 ) ) ;
#24770 = VECTOR ( 'NONE', #20306, 1000.000000000000000 ) ;
#24771 = DIRECTION ( 'NONE',  ( 0.000000000000000000, 1.000000000000000000, 0.000000000000000000 ) ) ;
#24772 = CARTESIAN_POINT ( 'NONE',  ( -0.7500000000000001110, 9.184850993605150903E-17, 17.00000000000000000 ) ) ;
#24773 = CARTESIAN_POINT ( 'NONE',  ( 18.73170057493538820, 18.73170057493532781, 13.33755215474602984 ) ) ;
#24774 = CARTESIAN_POINT ( 'NONE',  ( 3.756430356250004099, 29.22812499938548925, 6.831223922626973533 ) ) ;
#24775 = DIRECTION ( 'NONE',  ( 1.000000000000000000, 0.000000000000000000, 0.000000000000000000 ) ) ;
#24776 = CARTESIAN_POINT ( 'NONE',  ( 3.469446951953614189E-15, 35.50000000000000711, 8.999999999999992895 ) ) ;
#24777 = AXIS2_PLACEMENT_3D ( 'NONE', #12963, #7068, #24474 ) ;
#24778 = ORIENTED_EDGE ( 'NONE', *, *, #19593, .F. ) ;
#24779 = CARTESIAN_POINT ( 'NONE',  ( 4.000000000000003553, -8.999999999999992895, 4.893749998770967835 ) ) ;
#24780 = CARTESIAN_POINT ( 'NONE',  ( 2.000000000000003553, 25.91874999877097352, 5.535898384862238508 ) ) ;
#24781 = CARTESIAN_POINT ( 'NONE',  ( -1.878215178125004048, -28.36562499938548143, 5.746835883940462963 ) ) ;
#24782 = AXIS2_PLACEMENT_3D ( 'NONE', #8321, #14475, #18536 ) ;
#24783 = CARTESIAN_POINT ( 'NONE',  ( 0.000000000000000000, 0.000000000000000000, 15.00000000000000178 ) ) ;
#24784 = ADVANCED_FACE ( 'NONE', ( #20102 ), #5857, .F. ) ;
#24785 = CARTESIAN_POINT ( 'NONE',  ( -3.756430356249997882, 26.41562499938548569, 11.16877607737301226 ) ) ;
#24786 = CARTESIAN_POINT ( 'NONE',  ( 13.69242354489134073, -27.92360179968382283, -2.750000000000000000 ) ) ;
#24788 = VERTEX_POINT ( 'NONE', #21820 ) ;
#24787 = CARTESIAN_POINT ( 'NONE',  ( 0.000000000000000000, 0.000000000000000000, 1.000000000000000000 ) ) ;
#24789 = ORIENTED_EDGE ( 'NONE', *, *, #23372, .T. ) ;
#24790 = DIRECTION ( 'NONE',  ( 0.000000000000000000, 0.000000000000000000, -1.000000000000000000 ) ) ;
#24791 = CARTESIAN_POINT ( 'NONE',  ( 0.000000000000000000, 0.000000000000000000, -6.500000000000000000 ) ) ;
#24792 = ORIENTED_EDGE ( 'NONE', *, *, #25472, .T. ) ;
#24793 = CARTESIAN_POINT ( 'NONE',  ( -3.756430356250003211, -28.89062499938548356, 6.831223922626973533 ) ) ;
#24794 = FACE_OUTER_BOUND ( 'NONE', #6214, .T. ) ;
#24795 = CARTESIAN_POINT ( 'NONE',  ( -3.756430356250000546, 26.75312499938548783, 11.16877607737301048 ) ) ;
#24796 = VECTOR ( 'NONE', #21193, 1000.000000000000000 ) ;
#24797 = CARTESIAN_POINT ( 'NONE',  ( 3.469446951953614189E-15, 40.00000000000000000, 8.999999999999992895 ) ) ;
#24798 = CARTESIAN_POINT ( 'NONE',  ( -3.756430356249996105, 29.00312499938548427, 11.16877607737301226 ) ) ;
#24799 = CIRCLE ( 'NONE', #20192, 31.10000000000000142 ) ;
#24800 = CARTESIAN_POINT ( 'NONE',  ( 0.7500000000000000000, 0.000000000000000000, 17.69999999999999929 ) ) ;
#24801 = APPLICATION_CONTEXT ( 'automotive_design' ) ;
#24802 = CARTESIAN_POINT ( 'NONE',  ( 2.000000000000003997, -5.535898384862238508, 3.224999999999998757 ) ) ;
#24803 = DIRECTION ( 'NONE',  ( 0.000000000000000000, -1.000000000000000000, 0.000000000000000000 ) ) ;
#24804 =( BOUNDED_CURVE ( )  B_SPLINE_CURVE ( 2, ( #8452, #339, #18767, #18526, #6738, #6480, #16440, #24650, #2811 ),
 .UNSPECIFIED., .F., .F. ) 
 B_SPLINE_CURVE_WITH_KNOTS ( ( 3, 2, 2, 2, 3 ),
 ( 0.8250000000000000666, 0.8333333333333333703, 0.8499999999999999778, 0.8666666666666666963, 0.8750000000000000000 ),
 .UNSPECIFIED. ) 
 CURVE ( )  GEOMETRIC_REPRESENTATION_ITEM ( )  RATIONAL_B_SPLINE_CURVE ( ( 0.9330127018922194093, 0.9330127018922198534, 1.000000000000000000, 0.8660254037844387076, 1.000000000000000000, 0.8660254037844387076, 1.000000000000000000, 0.9330127018922194093, 0.9330127018922194093 ) ) 
 REPRESENTATION_ITEM ( '' )  );
#24805 = LINE ( 'NONE', #20619, #24614 ) ;
#24806 = CARTESIAN_POINT ( 'NONE',  ( -14.98253926456298579, 27.25313774936435962, 1.000000000000000000 ) ) ;
#24807 = CARTESIAN_POINT ( 'NONE',  ( 18.69544865292348490, 20.21119818077545460, 12.99999999999999467 ) ) ;
#24808 = DIRECTION ( 'NONE',  ( -0.9822872507286872779, 0.1873813145857327056, 0.000000000000000000 ) ) ;
#24809 = CARTESIAN_POINT ( 'NONE',  ( 18.11727402765218287, 23.42966878357085037, 6.831223922626973533 ) ) ;
#24810 = CARTESIAN_POINT ( 'NONE',  ( 18.73170057493538820, 18.73170057493532781, 13.33755215474602984 ) ) ;
#24811 = CARTESIAN_POINT ( 'NONE',  ( 4.000000000000003553, 27.70000000000000284, 8.999999999999992895 ) ) ;
#24812 = CARTESIAN_POINT ( 'NONE',  ( -3.999999999999996447, -8.999999999999992895, 18.00000000000000000 ) ) ;
#24813 =( BOUNDED_CURVE ( )  B_SPLINE_CURVE ( 2, ( #16214, #12290, #5888, #8238, #10190, #23935, #8 ),
 .UNSPECIFIED., .F., .F. ) 
 B_SPLINE_CURVE_WITH_KNOTS ( ( 3, 2, 2, 3 ),
 ( 0.2500000000000002776, 0.2666666666666669405, 0.2833333333333335480, 0.3000000000000002109 ),
 .UNSPECIFIED. ) 
 CURVE ( )  GEOMETRIC_REPRESENTATION_ITEM ( )  RATIONAL_B_SPLINE_CURVE ( ( 0.9999999999999977796, 0.8660254037844409281, 1.000000000000000000, 0.8660254037844387076, 1.000000000000000000, 0.8660254037844369313, 1.000000000000001776 ) ) 
 REPRESENTATION_ITEM ( '' )  );
#24814 = CARTESIAN_POINT ( 'NONE',  ( -1.878215178124995832, 27.99062499938548143, 5.746835883940462963 ) ) ;
#24815 = CARTESIAN_POINT ( 'NONE',  ( 0.000000000000000000, 0.000000000000000000, -6.500000000000000000 ) ) ;
#24816 =( GEOMETRIC_REPRESENTATION_CONTEXT ( 3 ) GLOBAL_UNCERTAINTY_ASSIGNED_CONTEXT ( ( #4955 ) ) GLOBAL_UNIT_ASSIGNED_CONTEXT ( ( #21934, #6103, #8201 ) ) REPRESENTATION_CONTEXT ( 'NONE', 'WORKASPACE' ) );
#24817 = DIRECTION ( 'NONE',  ( 0.000000000000000000, -0.000000000000000000, 1.000000000000000000 ) ) ;
#24818 = DIRECTION ( 'NONE',  ( -0.000000000000000000, -1.000000000000000000, -0.000000000000000000 ) ) ;
#24819 = VERTEX_POINT ( 'NONE', #16323 ) ;
#24820 = DIRECTION ( 'NONE',  ( -0.000000000000000000, 0.000000000000000000, 1.000000000000000000 ) ) ;
#24821 = CARTESIAN_POINT ( 'NONE',  ( -3.999999999999996003, 28.28124999877096712, 6.690598923241487306 ) ) ;
#24822 = CARTESIAN_POINT ( 'NONE',  ( 1.878215178124995832, -29.34062499938548285, 5.746835883940462963 ) ) ;
#24824 = ORIENTED_EDGE ( 'NONE', *, *, #907, .F. ) ;
#24823 = CARTESIAN_POINT ( 'NONE',  ( -3.999999999999996447, 25.22500000000000142, 8.999999999999992895 ) ) ;
#24825 = CARTESIAN_POINT ( 'NONE',  ( 15.94967733227004558, 21.60653158176235777, 11.30940107675849404 ) ) ;
#24826 = EDGE_CURVE ( 'NONE', #15121, #2787, #19296, .T. ) ;
#24827 = VERTEX_POINT ( 'NONE', #24292 ) ;
#24828 = CARTESIAN_POINT ( 'NONE',  ( 3.756430356249997882, -25.85312499938548925, 11.16877607737301226 ) ) ;
#24829 = VERTEX_POINT ( 'NONE', #14367 ) ;
#24830 = EDGE_LOOP ( 'NONE', ( #22610, #11235, #6178, #8287 ) ) ;
#24831 = ADVANCED_FACE ( 'NONE', ( #16185 ), #24151, .T. ) ;
#24832 = DIRECTION ( 'NONE',  ( -0.8443279255020122998, 0.5358267949790012086, 0.000000000000000000 ) ) ;
#24833 = CARTESIAN_POINT ( 'NONE',  ( -3.756430356249998326, 28.14062499938548356, 6.831223922626973533 ) ) ;
#24834 = FACE_OUTER_BOUND ( 'NONE', #8917, .T. ) ;
#24835 = ADVANCED_FACE ( 'NONE', ( #19840 ), #20349, .F. ) ;
#24836 = CARTESIAN_POINT ( 'NONE',  ( 1.878215178125000939, -12.25316411605952283, 2.878124999385483385 ) ) ;
#24837 = CARTESIAN_POINT ( 'NONE',  ( -3.020831617684079706, 38.79222141784235589, 4.157034316757149739 ) ) ;
#24838 = CARTESIAN_POINT ( 'NONE',  ( 2.672651547586948120E-15, 28.62812499938548783, 13.33755215474602984 ) ) ;
#24839 = CARTESIAN_POINT ( 'NONE',  ( 3.999999999999972466, -6.690598923241471319, 1.781249998770967125 ) ) ;
#24840 = DIRECTION ( 'NONE',  ( 1.000000000000000000, 0.000000000000000000, 0.000000000000000000 ) ) ;
#24841 = UNCERTAINTY_MEASURE_WITH_UNIT (LENGTH_MEASURE( 1.000000000000000082E-05 ), #15539, 'distance_accuracy_value', 'NONE');
#24842 = PRODUCT_DEFINITION_CONTEXT ( 'detailed design', #20643, 'design' ) ;
#24843 = CARTESIAN_POINT ( 'NONE',  ( -1.878215178124998497, 27.69062499938548427, 12.25316411605951927 ) ) ;
#24844 = DIRECTION ( 'NONE',  ( 0.000000000000000000, 0.000000000000000000, 1.000000000000000000 ) ) ;
#24845 = CARTESIAN_POINT ( 'NONE',  ( 0.000000000000000000, 0.000000000000000000, 1.000000000000000000 ) ) ;
#24846 = FACE_OUTER_BOUND ( 'NONE', #22701, .T. ) ;
#24847 = CARTESIAN_POINT ( 'NONE',  ( 17.42265644678770187, 18.93840597463967512, 12.99999999999999467 ) ) ;
#24848 = CARTESIAN_POINT ( 'NONE',  ( -1.878215178125004048, -26.67812499938548498, 5.746835883940462963 ) ) ;
#24849 = CARTESIAN_POINT ( 'NONE',  ( 3.756430356250004099, 26.19062499938548783, 6.831223922626973533 ) ) ;
#24850 = LINE ( 'NONE', #16746, #11204 ) ;
#24851 = CARTESIAN_POINT ( 'NONE',  ( 3.999999999999995559, -25.18750000000000000, 6.690598923241487306 ) ) ;
#24852 = LINE ( 'NONE', #21308, #21840 ) ;
#24853 = EDGE_LOOP ( 'NONE', ( #17012, #12597, #12459, #21835 ) ) ;
#24854 = CARTESIAN_POINT ( 'NONE',  ( 3.469446951953614189E-15, 40.00000000000000000, 4.999999999999992006 ) ) ;
#24856 = VERTEX_POINT ( 'NONE', #25862 ) ;
#24855 = FACE_OUTER_BOUND ( 'NONE', #19880, .T. ) ;
#24857 = ORIENTED_EDGE ( 'NONE', *, *, #15739, .F. ) ;
#24858 = ORIENTED_EDGE ( 'NONE', *, *, #23567, .F. ) ;
#24859 = ORIENTED_EDGE ( 'NONE', *, *, #22414, .F. ) ;
#24860 = VERTEX_POINT ( 'NONE', #5990 ) ;
#24861 = CARTESIAN_POINT ( 'NONE',  ( -3.834746474454188013E-15, -27.81249999999999645, 4.999999999999992006 ) ) ;
#24862 = ORIENTED_EDGE ( 'NONE', *, *, #7234, .F. ) ;
#24863 = EDGE_CURVE ( 'NONE', #19630, #12953, #8883, .T. ) ;
#24864 = DIRECTION ( 'NONE',  ( 0.000000000000000000, 0.000000000000000000, 1.000000000000000000 ) ) ;
#24865 = CARTESIAN_POINT ( 'NONE',  ( 3.756430356250002323, 29.71562499938548640, 11.16877607737301403 ) ) ;
#24866 = EDGE_CURVE ( 'NONE', #11133, #15750, #13420, .T. ) ;
#24867 = CARTESIAN_POINT ( 'NONE',  ( 3.756430356250004099, -6.831223922626973533, 0.6281249993854786107 ) ) ;
#24868 = FACE_BOUND ( 'NONE', #21347, .T. ) ;
#24869 = CARTESIAN_POINT ( 'NONE',  ( -2.000000000000003997, -25.46874999877096712, 5.535898384862238508 ) ) ;
#24870 = ADVANCED_FACE ( 'NONE', ( #16459 ), #2708, .T. ) ;
#24871 = CYLINDRICAL_SURFACE ( 'NONE', #19706, 0.5000000000000004441 ) ;
#24872 = CARTESIAN_POINT ( 'NONE',  ( 4.000000000000003553, -8.999999999999992895, 0.4499999999999990119 ) ) ;
#24873 = CIRCLE ( 'NONE', #23609, 0.5000000000000004441 ) ;
#24874 = CARTESIAN_POINT ( 'NONE',  ( -1.878215178124998497, -12.25316411605951927, 3.590624999385481075 ) ) ;
#24875 = AXIS2_PLACEMENT_3D ( 'NONE', #10722, #16511, #10996 ) ;
#24876 = CARTESIAN_POINT ( 'NONE',  ( -8.000000000000000000, 10.00000000000000178, 17.00000000000000000 ) ) ;
#24877 = CARTESIAN_POINT ( 'NONE',  ( -1.999999999999995781, -5.535898384862237620, 3.300000000000000711 ) ) ;
#24878 = CARTESIAN_POINT ( 'NONE',  ( -16.66421332384701515, -26.25859848311253941, -6.500000000000000000 ) ) ;
#24879 = CARTESIAN_POINT ( 'NONE',  ( 3.756430356250003655, -8.999999999999992895, 3.403124999385484628 ) ) ;
#24880 = CARTESIAN_POINT ( 'NONE',  ( -28.14012133169333651, -13.24173596767349359, -6.500000000000000000 ) ) ;
#24881 = EDGE_CURVE ( 'NONE', #10033, #23656, #16848, .T. ) ;
#24882 = CARTESIAN_POINT ( 'NONE',  ( -5.577813053751546416E-15, -25.33750000000000213, 12.99999999999999289 ) ) ;
#24883 = ORIENTED_EDGE ( 'NONE', *, *, #853, .T. ) ;
#24884 = EDGE_LOOP ( 'NONE', ( #15745, #17894, #20770, #9419 ) ) ;
#24885 = EDGE_LOOP ( 'NONE', ( #3167, #14661 ) ) ;
#24886 = CARTESIAN_POINT ( 'NONE',  ( -1.859271017917182139E-15, -27.08124999877096784, 12.99999999999999289 ) ) ;
#24887 = ORIENTED_EDGE ( 'NONE', *, *, #16972, .T. ) ;
#24888 = CIRCLE ( 'NONE', #19033, 0.4999999999999999445 ) ;
#24889 = CARTESIAN_POINT ( 'NONE',  ( -22.67092431280563503, 21.28941499438250062, 1.000000000000000000 ) ) ;
#24890 = VERTEX_POINT ( 'NONE', #18660 ) ;
#24891 = CARTESIAN_POINT ( 'NONE',  ( -13.24173596767398742, -28.14012133169310559, -6.500000000000000000 ) ) ;
#24892 = ADVANCED_FACE ( 'NONE', ( #16703, #6890 ), #14873, .F. ) ;
#24893 = ORIENTED_EDGE ( 'NONE', *, *, #4942, .T. ) ;
#24894 = DIRECTION ( 'NONE',  ( 0.000000000000000000, 0.000000000000000000, -1.000000000000000000 ) ) ;
#24895 = CARTESIAN_POINT ( 'NONE',  ( 3.735045420075836212E-15, 28.85312499938548569, 4.662447845253954171 ) ) ;
#24896 = DIRECTION ( 'NONE',  ( 0.000000000000000000, 0.000000000000000000, 1.000000000000000000 ) ) ;
#24897 = EDGE_CURVE ( 'NONE', #15816, #22149, #25647, .T. ) ;
#24898 = CARTESIAN_POINT ( 'NONE',  ( -3.137519842735244810E-15, 26.46249999999999858, 4.999999999999991118 ) ) ;
#24899 = FACE_OUTER_BOUND ( 'NONE', #21595, .T. ) ;
#24900 = CARTESIAN_POINT ( 'NONE',  ( 22.42204162038009230, 17.10964686446126848, 8.999999999999992895 ) ) ;
#24901 = CARTESIAN_POINT ( 'NONE',  ( -1.999999999999995781, 28.30000000000000071, 5.535898384862237620 ) ) ;
#24902 = CARTESIAN_POINT ( 'NONE',  ( 2.000000000000003997, 25.07499999999999929, 5.535898384862238508 ) ) ;
#24903 = ADVANCED_FACE ( 'NONE', ( #18791 ), #879, .F. ) ;
#24904 = CARTESIAN_POINT ( 'NONE',  ( 22.44855812467459089, 17.13616336875576351, 6.831223922626973533 ) ) ;
#24905 = CYLINDRICAL_SURFACE ( 'NONE', #4076, 31.10000000000000142 ) ;
#24906 = EDGE_LOOP ( 'NONE', ( #9112, #8107, #15569, #17038, #17421 ) ) ;
#24907 = PRODUCT_DEFINITION_SHAPE ( 'NONE', 'NONE',  #25881 ) ;
#24908 = CARTESIAN_POINT ( 'NONE',  ( 2.000000000000000000, 27.56874999877097210, 12.46410161513774817 ) ) ;
#24909 = CARTESIAN_POINT ( 'NONE',  ( -3.756430356250003211, -26.97812499938547859, 6.831223922626973533 ) ) ;
#24910 = LINE ( 'NONE', #1103, #18781 ) ;
#24911 = CARTESIAN_POINT ( 'NONE',  ( 4.000000000000003553, 29.48124999877096997, 6.690598923241489970 ) ) ;
#24912 = CARTESIAN_POINT ( 'NONE',  ( 4.000000000000002665, 29.87009603951200276, 10.45670610619353980 ) ) ;
#24914 = ORIENTED_EDGE ( 'NONE', *, *, #6019, .T. ) ;
#24913 = CARTESIAN_POINT ( 'NONE',  ( -1.878215178124998275, 29.60312499938548925, 12.25316411605951927 ) ) ;
#24915 = EDGE_LOOP ( 'NONE', ( #19825, #11824, #753, #17395 ) ) ;
#24916 = LINE ( 'NONE', #14976, #17490 ) ;
#24917 = CARTESIAN_POINT ( 'NONE',  ( 4.000000000000003553, 26.29374999877096997, 8.999999999999992895 ) ) ;
#24918 = VERTEX_POINT ( 'NONE', #18546 ) ;
#24919 = CARTESIAN_POINT ( 'NONE',  ( 1.859271017917182139E-15, 25.78750000000000142, 12.99999999999999289 ) ) ;
#24920 = LINE ( 'NONE', #20609, #18065 ) ;
#24921 = CARTESIAN_POINT ( 'NONE',  ( -1.878215178124994722, 25.29062499938548925, 5.746835883940462963 ) ) ;
#24922 = CARTESIAN_POINT ( 'NONE',  ( 2.451530025009136970, 31.00322564728514152, -6.500000000000000000 ) ) ;
#24923 = CARTESIAN_POINT ( 'NONE',  ( -3.756430356249996105, 28.92812499938548498, 6.831223922626973533 ) ) ;
#24924 = EDGE_CURVE ( 'NONE', #14667, #4479, #12906, .T. ) ;
#24925 = CARTESIAN_POINT ( 'NONE',  ( 4.000000000000000888, 28.95624999877097494, 11.30940107675849760 ) ) ;
#24926 = FILL_AREA_STYLE ('',( #738 ) ) ;
#24927 = DIRECTION ( 'NONE',  ( 0.8090169943749532244, 0.5877852522924652545, 0.000000000000000000 ) ) ;
#24928 = FACE_OUTER_BOUND ( 'NONE', #24304, .T. ) ;
#24929 = CARTESIAN_POINT ( 'NONE',  ( -1.878215178124995832, 27.99062499938548143, 5.746835883940462963 ) ) ;
#24930 = CARTESIAN_POINT ( 'NONE',  ( 21.71259759894040187, 16.05574334944795112, 11.30940107675849760 ) ) ;
#24931 = CARTESIAN_POINT ( 'NONE',  ( 17.48087792458429135, 22.79327268050296240, 6.831223922626973533 ) ) ;
#24932 = CARTESIAN_POINT ( 'NONE',  ( 20.89942480057588270, 20.89942480057580099, 4.381197846482986158 ) ) ;
#24933 = PLANE ( 'NONE',  #16344 ) ;
#24934 = CARTESIAN_POINT ( 'NONE',  ( -1.878215178124998497, 26.79062499938548214, 12.25316411605951927 ) ) ;
#24935 = CARTESIAN_POINT ( 'NONE',  ( 23.85222316637486273, 18.19536891688240843, 8.735714247490120599 ) ) ;
#24936 = CARTESIAN_POINT ( 'NONE',  ( 20.96136040992792715, 18.30516303196848327, 12.25316411605952283 ) ) ;
#24937 = DIRECTION ( 'NONE',  ( 0.000000000000000000, 0.000000000000000000, -1.000000000000000000 ) ) ;
#24938 = ORIENTED_EDGE ( 'NONE', *, *, #16, .T. ) ;
#24939 = CARTESIAN_POINT ( 'NONE',  ( -1.057460391440397258E-14, 28.71250000000000213, 4.999999999999992006 ) ) ;
#24940 = CARTESIAN_POINT ( 'NONE',  ( 2.620986760973688460E-15, 27.98124999877096997, 13.61880215351699874 ) ) ;
#24941 = CARTESIAN_POINT ( 'NONE',  ( -3.756430356250003655, -28.74062499938548498, 8.999999999999992895 ) ) ;
#24943 = EDGE_LOOP ( 'NONE', ( #4697, #14940, #20856, #16973 ) ) ;
#24942 = CARTESIAN_POINT ( 'NONE',  ( -31.03863125411927371, -1.952785157361310198, -6.500000000000000000 ) ) ;
#24944 = CARTESIAN_POINT ( 'NONE',  ( -3.756430356249996994, 26.82812499938548711, 8.999999999999992895 ) ) ;
#24945 = VERTEX_POINT ( 'NONE', #22726 ) ;
#24946 = CARTESIAN_POINT ( 'NONE',  ( -3.735045420075836212E-15, -27.50312499938548783, 4.662447845253954171 ) ) ;
#24947 = VERTEX_POINT ( 'NONE', #628 ) ;
#24948 = ORIENTED_EDGE ( 'NONE', *, *, #23689, .T. ) ;
#24949 = CARTESIAN_POINT ( 'NONE',  ( 19.74889435023732887, 22.58381402607102473, 5.528701699505818468 ) ) ;
#24950 = CARTESIAN_POINT ( 'NONE',  ( 1.878215178125008489, 27.57812499938549422, 5.746835883940462963 ) ) ;
#24951 = DIRECTION ( 'NONE',  ( 1.000000000000000000, 0.000000000000000000, 0.000000000000000000 ) ) ;
#24952 =( BOUNDED_CURVE ( )  B_SPLINE_CURVE ( 2, ( #7024, #25077, #21153, #11196, #21532, #7295, #11583, #11077, #19556, #11467, #23122, #19176, #11334, #23239, #19438, #5322, #17481, #19055, #23499, #1273, #5205, #17366, #1140, #13302, #9113, #1529, #13183, #25332, #3224, #1658, #9257, #17245, #15391, #17102, #7163, #3614, #25453, #25215, #5452, #16979, #15272, #21275, #24944, #22991, #3359, #19317, #1412, #13444, #9499, #21414, #7538, #15533, #5076, #13056, #25841, #22040, #19940, #8066, #20205, #218, #19821, #15912, #5703, #9635, #19698, #11968, #7924, #15659, #17613, #1797, #23625, #21920, #6215, #2043, #7674, #6090, #25714, #4002, #10011, #16048, #18006, #10141, #2180, #20078, #17869, #13682, #12238, #21796, #4124, #23744, #21655, #8188, #24129, #1922, #14075, #23885, #18145, #16166, #14206, #12102, #22179, #5969, #9766, #4264, #25591, #3738, #24010, #94, #11721, #17744, #15775, #7796, #5831, #13818, #3879, #11850, #9883, #13952, #4904, #8579, #728 ),
 .UNSPECIFIED., .F., .F. ) 
 B_SPLINE_CURVE_WITH_KNOTS ( ( 3, 2, 2, 2, 2, 2, 2, 2, 2, 2, 2, 2, 2, 2, 2, 2, 2, 2, 2, 2, 2, 2, 2, 2, 2, 2, 2, 2, 2, 2, 2, 2, 2, 2, 2, 2, 2, 2, 2, 2, 2, 2, 2, 2, 2, 2, 2, 2, 2, 2, 2, 2, 2, 2, 2, 2, 2, 2, 2, 2, 3 ),
 ( 0.000000000000000000, 0.01666666666666666644, 0.03333333333333333287, 0.05000000000000000278, 0.06666666666666666574, 0.08333333333333332871, 0.1000000000000000056, 0.1166666666666666685, 0.1333333333333333315, 0.1499999999999999944, 0.1666666666666666574, 0.1833333333333333204, 0.2000000000000000111, 0.2166666666666666741, 0.2333333333333333370, 0.2500000000000000000, 0.2666666666666666630, 0.2833333333333333259, 0.2999999999999999889, 0.3166666666666666519, 0.3333333333333333148, 0.3499999999999999778, 0.3666666666666666408, 0.3833333333333333592, 0.4000000000000000222, 0.4166666666666666852, 0.4333333333333333481, 0.4500000000000000111, 0.4666666666666666741, 0.4833333333333333370, 0.5000000000000000000, 0.5166666666666667185, 0.5333333333333333259, 0.5500000000000000444, 0.5666666666666666519, 0.5833333333333333703, 0.5999999999999999778, 0.6166666666666666963, 0.6333333333333333037, 0.6500000000000000222, 0.6666666666666666297, 0.6833333333333333481, 0.6999999999999999556, 0.7166666666666666741, 0.7333333333333332815, 0.7500000000000000000, 0.7666666666666667185, 0.7833333333333333259, 0.8000000000000000444, 0.8166666666666666519, 0.8333333333333333703, 0.8499999999999999778, 0.8666666666666666963, 0.8833333333333333037, 0.9000000000000000222, 0.9166666666666666297, 0.9333333333333333481, 0.9499999999999999556, 0.9666666666666666741, 0.9833333333333332815, 1.000000000000000000 ),
 .UNSPECIFIED. ) 
 CURVE ( )  GEOMETRIC_REPRESENTATION_ITEM ( )  RATIONAL_B_SPLINE_CURVE ( ( 1.000000000000000000, 0.8660254037844387076, 1.000000000000000000, 0.8660254037844387076, 1.000000000000000000, 0.8660254037844387076, 1.000000000000000000, 0.8660254037844387076, 1.000000000000000000, 0.8660254037844387076, 1.000000000000000000, 0.8660254037844387076, 1.000000000000000000, 0.8660254037844387076, 1.000000000000000000, 0.8660254037844387076, 1.000000000000000000, 0.8660254037844387076, 1.000000000000000000, 0.8660254037844387076, 1.000000000000000000, 0.8660254037844387076, 1.000000000000000000, 0.8660254037844387076, 1.000000000000000000, 0.8660254037844387076, 1.000000000000000000, 0.8660254037844387076, 1.000000000000000000, 0.8660254037844387076, 1.000000000000000000, 0.8660254037844387076, 1.000000000000000000, 0.8660254037844387076, 1.000000000000000000, 0.8660254037844387076, 1.000000000000000000, 0.8660254037844387076, 1.000000000000000000, 0.8660254037844387076, 1.000000000000000000, 0.8660254037844387076, 1.000000000000000000, 0.8660254037844387076, 1.000000000000000000, 0.8660254037844387076, 1.000000000000000000, 0.8660254037844387076, 1.000000000000000000, 0.8660254037844387076, 1.000000000000000000, 0.8660254037844387076, 1.000000000000000000, 0.8660254037844387076, 1.000000000000000000, 0.8660254037844387076, 1.000000000000000000, 0.8660254037844387076, 1.000000000000000000, 0.8660254037844387076, 1.000000000000000000, 0.8660254037844387076, 1.000000000000000000, 0.8660254037844387076, 1.000000000000000000, 0.8660254037844387076, 1.000000000000000000, 0.8660254037844387076, 1.000000000000000000, 0.8660254037844387076, 1.000000000000000000, 0.8660254037844387076, 1.000000000000000000, 0.8660254037844387076, 1.000000000000000000, 0.8660254037844387076, 1.000000000000000000, 0.8660254037844387076, 1.000000000000000000, 0.8660254037844387076, 1.000000000000000000, 0.8660254037844387076, 1.000000000000000000, 0.8660254037844387076, 1.000000000000000000, 0.8660254037844387076, 1.000000000000000000, 0.8660254037844387076, 1.000000000000000000, 0.8660254037844387076, 1.000000000000000000, 0.8660254037844387076, 1.000000000000000000, 0.8660254037844387076, 1.000000000000000000, 0.8660254037844387076, 1.000000000000000000, 0.8660254037844387076, 1.000000000000000000, 0.8660254037844387076, 1.000000000000000000, 0.8660254037844387076, 1.000000000000000000, 0.8660254037844387076, 1.000000000000000000, 0.8660254037844387076, 1.000000000000000000, 0.8660254037844387076, 1.000000000000000000, 0.8660254037844387076, 1.000000000000000000, 0.8660254037844387076, 1.000000000000000000, 0.8660254037844387076, 1.000000000000000000, 0.8660254037844387076, 1.000000000000000000, 0.8660254037844387076, 1.000000000000000000, 0.8660254037844387076, 1.000000000000000000 ) ) 
 REPRESENTATION_ITEM ( '' )  );
#24953 = EDGE_CURVE ( 'NONE', #21593, #19594, #13037, .T. ) ;
#24954 = CARTESIAN_POINT ( 'NONE',  ( 2.000000000000003997, 29.06874999877096855, 5.535898384862238508 ) ) ;
#24955 = CARTESIAN_POINT ( 'NONE',  ( -1.859271017917182139E-15, -27.08124999877096784, 12.99999999999999289 ) ) ;
#24956 =( BOUNDED_CURVE ( )  B_SPLINE_CURVE ( 2, ( #1916, #23619, #1652, #13437, #7532, #19548, #9628, #9877, #15653 ),
 .UNSPECIFIED., .F., .F. ) 
 B_SPLINE_CURVE_WITH_KNOTS ( ( 3, 2, 2, 2, 3 ),
 ( 0.07500000000000001110, 0.08333333333333332871, 0.1000000000000000056, 0.1166666666666666685, 0.1250000000000000000 ),
 .UNSPECIFIED. ) 
 CURVE ( )  GEOMETRIC_REPRESENTATION_ITEM ( )  RATIONAL_B_SPLINE_CURVE ( ( 0.9330127018922192983, 0.9330127018922194093, 1.000000000000000000, 0.8660254037844387076, 1.000000000000000000, 0.8660254037844387076, 1.000000000000000000, 0.9330127018922194093, 0.9330127018922194093 ) ) 
 REPRESENTATION_ITEM ( '' )  );
#24957 = CARTESIAN_POINT ( 'NONE',  ( -3.756430356249996994, 28.51562499938548356, 8.999999999999992895 ) ) ;
#24958 = EDGE_CURVE ( 'NONE', #125, #5938, #13128, .T. ) ;
#24959 = CARTESIAN_POINT ( 'NONE',  ( -1.999999999999995781, -5.535898384862237620, 1.893749998770968723 ) ) ;
#24960 = CARTESIAN_POINT ( 'NONE',  ( 3.752267015613588906E-15, -4.381197846482986158, 3.712500000000000355 ) ) ;
#24961 = CARTESIAN_POINT ( 'NONE',  ( -1.878215178124998497, 29.04062499938548569, 12.25316411605951927 ) ) ;
#24962 = CARTESIAN_POINT ( 'NONE',  ( 0.000000000000000000, 0.000000000000000000, -6.500000000000000000 ) ) ;
#24963 = DIRECTION ( 'NONE',  ( 0.000000000000000000, 0.000000000000000000, 1.000000000000000000 ) ) ;
#24964 = EDGE_CURVE ( 'NONE', #22864, #1602, #20487, .T. ) ;
#24965 = DIRECTION ( 'NONE',  ( 0.000000000000000000, 0.000000000000000000, 1.000000000000000000 ) ) ;
#24966 = CARTESIAN_POINT ( 'NONE',  ( 3.756430356249995661, -28.14062499938548356, 6.831223922626973533 ) ) ;
#24967 = FACE_OUTER_BOUND ( 'NONE', #2987, .T. ) ;
#24968 = DIRECTION ( 'NONE',  ( 0.000000000000000000, 0.000000000000000000, -1.000000000000000000 ) ) ;
#24969 = CARTESIAN_POINT ( 'NONE',  ( 4.000000000000003553, 27.25000000000000000, 8.999999999999992895 ) ) ;
#24970 = DIRECTION ( 'NONE',  ( 0.000000000000000000, 0.000000000000000000, -1.000000000000000000 ) ) ;
#24971 = VERTEX_POINT ( 'NONE', #12245 ) ;
#24972 = EDGE_CURVE ( 'NONE', #15499, #21679, #18476, .T. ) ;
#24973 = DIRECTION ( 'NONE',  ( 0.4257792915650852050, 0.9048270524660135816, 0.000000000000000000 ) ) ;
#24975 = EDGE_LOOP ( 'NONE', ( #21182, #6124 ) ) ;
#24974 = CARTESIAN_POINT ( 'NONE',  ( -10.94867358849371541, -28.91604871112453168, -6.500000000000000000 ) ) ;
#24976 = ORIENTED_EDGE ( 'NONE', *, *, #18142, .F. ) ;
#24977 = CIRCLE ( 'NONE', #17048, 31.10000000000000142 ) ;
#24978 = ORIENTED_EDGE ( 'NONE', *, *, #16544, .F. ) ;
#24979 = EDGE_LOOP ( 'NONE', ( #8970, #24498, #12632, #2520 ) ) ;
#24980 = ORIENTED_EDGE ( 'NONE', *, *, #14571, .F. ) ;
#24981 = DIRECTION ( 'NONE',  ( 0.5877852522924730261, -0.8090169943749474513, 0.000000000000000000 ) ) ;
#24982 = CYLINDRICAL_SURFACE ( 'NONE', #21125, 4.000000000000000000 ) ;
#24984 = ORIENTED_EDGE ( 'NONE', *, *, #10657, .T. ) ;
#24983 = CIRCLE ( 'NONE', #22894, 31.10000000000000142 ) ;
#24985 = CARTESIAN_POINT ( 'NONE',  ( 1.878215178125000939, 29.67812499938548498, 12.25316411605952283 ) ) ;
#24986 = CARTESIAN_POINT ( 'NONE',  ( -3.756430356249995661, -6.831223922626973533, 0.7781249993854825187 ) ) ;
#24987 =( NAMED_UNIT ( * ) PLANE_ANGLE_UNIT ( ) SI_UNIT ( $, .RADIAN. ) );
#24988 = CARTESIAN_POINT ( 'NONE',  ( 4.000000000000003553, -8.999999999999992895, 2.643749998770966059 ) ) ;
#24989 = CARTESIAN_POINT ( 'NONE',  ( -5.706339097770898761, 29.50000000000000000, 10.85410196624973800 ) ) ;
#24990 = EDGE_CURVE ( 'NONE', #15349, #11855, #10269, .T. ) ;
#24991 = CARTESIAN_POINT ( 'NONE',  ( 3.403349963601436823, -25.83240171513484995, 20.00001200000000878 ) ) ;
#24992 = CARTESIAN_POINT ( 'NONE',  ( 3.756430356250002323, -11.16877607737301226, 3.703124999385482674 ) ) ;
#24993 = PRODUCT_DEFINITION ( 'UNKNOWN', '', #6035, #23010 ) ;
#24994 = FACE_OUTER_BOUND ( 'NONE', #25076, .T. ) ;
#24995 = CARTESIAN_POINT ( 'NONE',  ( 0.000000000000000000, 0.000000000000000000, 17.00000000000000000 ) ) ;
#24996 = DIRECTION ( 'NONE',  ( 1.000000000000000000, 0.000000000000000000, 0.000000000000000000 ) ) ;
#24997 = CARTESIAN_POINT ( 'NONE',  ( -31.09598070739550835, -0.4999838450256507416, -6.500000000000000000 ) ) ;
#24998 = CARTESIAN_POINT ( 'NONE',  ( 2.672651547586948120E-15, -13.33755215474603162, 4.640624999385483562 ) ) ;
#24999 = CARTESIAN_POINT ( 'NONE',  ( -30.00000000000000355, 0.000000000000000000, 0.000000000000000000 ) ) ;
#25000 = AXIS2_PLACEMENT_3D ( 'NONE', #1295, #11484, #25232 ) ;
#25001 = FACE_OUTER_BOUND ( 'NONE', #17972, .T. ) ;
#25002 = ORIENTED_EDGE ( 'NONE', *, *, #25288, .F. ) ;
#25003 = EDGE_CURVE ( 'NONE', #16624, #13717, #10118, .T. ) ;
#25004 = EDGE_LOOP ( 'NONE', ( #24540, #24105, #13530, #21986 ) ) ;
#25005 = EDGE_CURVE ( 'NONE', #8582, #15499, #4131, .T. ) ;
#25006 = EDGE_LOOP ( 'NONE', ( #24859, #856, #1201, #13894 ) ) ;
#25007 = CARTESIAN_POINT ( 'NONE',  ( -30.10000000000000142, 3.686186865433532535E-15, -6.500000000000000000 ) ) ;
#25008 = ORIENTED_EDGE ( 'NONE', *, *, #9035, .T. ) ;
#25009 = CARTESIAN_POINT ( 'NONE',  ( -1.878215178125004048, -26.67812499938548498, 5.746835883940462963 ) ) ;
#25010 = ORIENTED_EDGE ( 'NONE', *, *, #19431, .T. ) ;
#25011 = CARTESIAN_POINT ( 'NONE',  ( -3.999999999999999112, 27.90624999877098134, 11.30940107675849404 ) ) ;
#25012 = VECTOR ( 'NONE', #11157, 1000.000000000000000 ) ;
#25013 = ORIENTED_EDGE ( 'NONE', *, *, #24631, .F. ) ;
#25014 = AXIS2_PLACEMENT_3D ( 'NONE', #2828, #14607, #8470 ) ;
#25015 = DIRECTION ( 'NONE',  ( 1.000000000000000000, 0.000000000000000000, 0.000000000000000000 ) ) ;
#25016 = CARTESIAN_POINT ( 'NONE',  ( 1.878215178125004048, 28.36562499938548143, 5.746835883940462963 ) ) ;
#25017 = CARTESIAN_POINT ( 'NONE',  ( 1.071796769724492338, 27.10134618820329777, 12.99999999999999467 ) ) ;
#25018 = AXIS2_PLACEMENT_3D ( 'NONE', #17338, #13153, #8972 ) ;
#25019 = AXIS2_PLACEMENT_3D ( 'NONE', #15837, #1974, #9941 ) ;
#25020 = DIRECTION ( 'NONE',  ( 0.000000000000000000, 0.000000000000000000, 1.000000000000000000 ) ) ;
#25021 = LINE ( 'NONE', #7109, #2483 ) ;
#25022 = CARTESIAN_POINT ( 'NONE',  ( 21.44093096148375466, 16.12853620556493794, 11.16877607737301226 ) ) ;
#25023 = DIRECTION ( 'NONE',  ( 0.000000000000000000, 0.000000000000000000, -1.000000000000000000 ) ) ;
#25024 = CARTESIAN_POINT ( 'NONE',  ( 2.672651547586948120E-15, 29.52812499938548285, 13.33755215474602984 ) ) ;
#25025 = CARTESIAN_POINT ( 'NONE',  ( 18.64987758779700044, 21.30607496575630222, 12.25316411605951927 ) ) ;
#25026 = DIRECTION ( 'NONE',  ( -0.000000000000000000, 0.000000000000000000, 1.000000000000000000 ) ) ;
#25027 = VECTOR ( 'NONE', #6123, 1000.000000000000000 ) ;
#25028 = EDGE_CURVE ( 'NONE', #22241, #25114, #2410, .T. ) ;
#25029 = ORIENTED_EDGE ( 'NONE', *, *, #7524, .T. ) ;
#25030 = CARTESIAN_POINT ( 'NONE',  ( 2.000000000000005329, 28.61874999877097281, 5.535898384862238508 ) ) ;
#25031 = SHAPE_REPRESENTATION ( 'MAS-166', ( #5624, #14799, #25251, #11867, #6445, #23581, #9377, #11032, #15651, #20222, #4351 ), #1016 ) ;
#25034 = ADVANCED_FACE ( 'NONE', ( #489 ), #24137, .F. ) ;
#25033 = CARTESIAN_POINT ( 'NONE',  ( 1.878215178124998497, -28.14062499938548356, 12.25316411605951927 ) ) ;
#25032 = VECTOR ( 'NONE', #21875, 1000.000000000000000 ) ;
#25035 = CARTESIAN_POINT ( 'NONE',  ( 17.08421000182759997, -25.98730014090448392, -6.500000000000000000 ) ) ;
#25036 = CIRCLE ( 'NONE', #2919, 0.5000000000000000000 ) ;
#25037 = CARTESIAN_POINT ( 'NONE',  ( 3.735045420075836212E-15, 27.16562499938548569, 4.662447845253954171 ) ) ;
#25038 = FACE_OUTER_BOUND ( 'NONE', #2605, .T. ) ;
#25040 = ORIENTED_EDGE ( 'NONE', *, *, #998, .T. ) ;
#25039 = CARTESIAN_POINT ( 'NONE',  ( -3.756430356249996549, 29.49062499938548854, 6.831223922626973533 ) ) ;
#25041 = ORIENTED_EDGE ( 'NONE', *, *, #23089, .F. ) ;
#25042 = FACE_OUTER_BOUND ( 'NONE', #1985, .T. ) ;
#25043 = CARTESIAN_POINT ( 'NONE',  ( 4.000000000000001776, 26.25624999877096855, 11.30940107675849760 ) ) ;
#25044 = VECTOR ( 'NONE', #1200, 1000.000000000000000 ) ;
#25045 = VERTEX_POINT ( 'NONE', #14593 ) ;
#25046 = CARTESIAN_POINT ( 'NONE',  ( -3.756430356250003211, -28.44062499938548427, 6.831223922626973533 ) ) ;
#25047 = CARTESIAN_POINT ( 'NONE',  ( 3.756430356250004543, 29.22812499938548925, 6.831223922626973533 ) ) ;
#25048 = CARTESIAN_POINT ( 'NONE',  ( -3.756430356249996549, 25.77812499938548285, 6.831223922626973533 ) ) ;
#25049 = CIRCLE ( 'NONE', #16689, 0.5000000000000001110 ) ;
#25050 = CIRCLE ( 'NONE', #5834, 0.5000000000000003331 ) ;
#25051 = CARTESIAN_POINT ( 'NONE',  ( 22.44180146790808905, 16.78494721841563475, 6.690598923241489970 ) ) ;
#25052 = CARTESIAN_POINT ( 'NONE',  ( 3.756430356250004543, 29.22812499938548925, 6.831223922626973533 ) ) ;
#25053 = VECTOR ( 'NONE', #18021, 1000.000000000000000 ) ;
#25054 = AXIS2_PLACEMENT_3D ( 'NONE', #2912, #5145, #19114 ) ;
#25055 = ITEM_DEFINED_TRANSFORMATION ( 'NONE', 'NONE', #14799,  #21036 ) ;
#25056 = DIRECTION ( 'NONE',  ( -0.000000000000000000, -0.000000000000000000, -1.000000000000000000 ) ) ;
#25057 = DIRECTION ( 'NONE',  ( -0.000000000000000000, -0.000000000000000000, 1.000000000000000000 ) ) ;
#25058 = CARTESIAN_POINT ( 'NONE',  ( 2.672651547586948120E-15, 26.37812499938548427, 13.33755215474603162 ) ) ;
#25059 = CIRCLE ( 'NONE', #9601, 0.5000000000000003331 ) ;
#25060 = LINE ( 'NONE', #9099, #24169 ) ;
#25061 = CARTESIAN_POINT ( 'NONE',  ( 18.88852612644745932, 21.54472350440676109, 12.25316411605951927 ) ) ;
#25062 = CARTESIAN_POINT ( 'NONE',  ( 18.12403068441868470, 23.78088493391098979, 6.690598923241487306 ) ) ;
#25063 = EDGE_CURVE ( 'NONE', #10717, #3169, #12494, .T. ) ;
#25064 = CARTESIAN_POINT ( 'NONE',  ( 17.20921128712764414, 22.86606553661995278, 6.690598923241487306 ) ) ;
#25065 = CARTESIAN_POINT ( 'NONE',  ( -3.756430356249997882, 27.20312499938548001, 11.16877607737301226 ) ) ;
#25066 = CIRCLE ( 'NONE', #6675, 31.10000000000000142 ) ;
#25067 = DIRECTION ( 'NONE',  ( 1.000000000000000000, 0.000000000000000000, 0.000000000000000000 ) ) ;
#25068 =( BOUNDED_CURVE ( )  B_SPLINE_CURVE ( 2, ( #15866, #13910, #17707, #14162, #1756, #23583, #5784, #21880, #13771, #3832, #11811, #3964, #23837, #11929, #19898, #22665, #20415, #2516, #10736, #4605, #439, #4348, #10615, #14306, #16640, #24608, #8409, #10485, #8272, #24224, #14545, #18485, #573, #8543, #16524, #4471, #12446, #18608, #22388, #6311, #10341, #22269, #12324, #20817, #12843, #22525, #8792, #2387, #14817, #2901, #24750, #16782, #12587, #24484, #4866, #12723, #6834, #6564, #20293, #6692, #20565, #2654, #10868, #22790, #694, #18342, #16396, #20692, #8658, #18868, #24366, #14686, #4753, #18722, #2774, #6442, #14427, #814, #16254, #14937, #13365, #3041, #20960, #5376, #24879, #1340, #21337, #23049, #7465, #11011, #13114, #5136, #3420, #7345, #9049, #16914, #15074, #1194, #22912, #11396, #6958, #18991, #19370, #4997, #9313, #1464, #9436, #17417, #17298, #25380, #12977, #21203, #1075, #13501, #15456, #17031, #23425, #24998, #7086, #21085, #9175 ),
 .UNSPECIFIED., .F., .F. ) 
 B_SPLINE_CURVE_WITH_KNOTS ( ( 3, 2, 2, 2, 2, 2, 2, 2, 2, 2, 2, 2, 2, 2, 2, 2, 2, 2, 2, 2, 2, 2, 2, 2, 2, 2, 2, 2, 2, 2, 2, 2, 2, 2, 2, 2, 2, 2, 2, 2, 2, 2, 2, 2, 2, 2, 2, 2, 2, 2, 2, 2, 2, 2, 2, 2, 2, 2, 2, 2, 3 ),
 ( 0.000000000000000000, 0.01666666666666666644, 0.03333333333333333287, 0.05000000000000000278, 0.06666666666666666574, 0.08333333333333332871, 0.1000000000000000056, 0.1166666666666666685, 0.1333333333333333315, 0.1499999999999999944, 0.1666666666666666574, 0.1833333333333333204, 0.2000000000000000111, 0.2166666666666666741, 0.2333333333333333370, 0.2500000000000000000, 0.2666666666666666630, 0.2833333333333333259, 0.2999999999999999889, 0.3166666666666666519, 0.3333333333333333148, 0.3499999999999999778, 0.3666666666666666408, 0.3833333333333333592, 0.4000000000000000222, 0.4166666666666666852, 0.4333333333333333481, 0.4500000000000000111, 0.4666666666666666741, 0.4833333333333333370, 0.5000000000000000000, 0.5166666666666667185, 0.5333333333333333259, 0.5500000000000000444, 0.5666666666666666519, 0.5833333333333333703, 0.5999999999999999778, 0.6166666666666666963, 0.6333333333333333037, 0.6500000000000000222, 0.6666666666666666297, 0.6833333333333333481, 0.6999999999999999556, 0.7166666666666666741, 0.7333333333333332815, 0.7500000000000000000, 0.7666666666666667185, 0.7833333333333333259, 0.8000000000000000444, 0.8166666666666666519, 0.8333333333333333703, 0.8499999999999999778, 0.8666666666666666963, 0.8833333333333333037, 0.9000000000000000222, 0.9166666666666666297, 0.9333333333333333481, 0.9499999999999999556, 0.9666666666666666741, 0.9833333333333332815, 1.000000000000000000 ),
 .UNSPECIFIED. ) 
 CURVE ( )  GEOMETRIC_REPRESENTATION_ITEM ( )  RATIONAL_B_SPLINE_CURVE ( ( 1.000000000000000000, 0.8660254037844387076, 1.000000000000000000, 0.8660254037844387076, 1.000000000000000000, 0.8660254037844387076, 1.000000000000000000, 0.8660254037844387076, 1.000000000000000000, 0.8660254037844387076, 1.000000000000000000, 0.8660254037844387076, 1.000000000000000000, 0.8660254037844387076, 1.000000000000000000, 0.8660254037844387076, 1.000000000000000000, 0.8660254037844387076, 1.000000000000000000, 0.8660254037844387076, 1.000000000000000000, 0.8660254037844387076, 1.000000000000000000, 0.8660254037844387076, 1.000000000000000000, 0.8660254037844387076, 1.000000000000000000, 0.8660254037844387076, 1.000000000000000000, 0.8660254037844387076, 1.000000000000000000, 0.8660254037844387076, 1.000000000000000000, 0.8660254037844387076, 1.000000000000000000, 0.8660254037844387076, 1.000000000000000000, 0.8660254037844387076, 1.000000000000000000, 0.8660254037844387076, 1.000000000000000000, 0.8660254037844387076, 1.000000000000000000, 0.8660254037844387076, 1.000000000000000000, 0.8660254037844387076, 1.000000000000000000, 0.8660254037844387076, 1.000000000000000000, 0.8660254037844387076, 1.000000000000000000, 0.8660254037844387076, 1.000000000000000000, 0.8660254037844387076, 1.000000000000000000, 0.8660254037844387076, 1.000000000000000000, 0.8660254037844387076, 1.000000000000000000, 0.8660254037844387076, 1.000000000000000000, 0.8660254037844387076, 1.000000000000000000, 0.8660254037844387076, 1.000000000000000000, 0.8660254037844387076, 1.000000000000000000, 0.8660254037844387076, 1.000000000000000000, 0.8660254037844387076, 1.000000000000000000, 0.8660254037844387076, 1.000000000000000000, 0.8660254037844387076, 1.000000000000000000, 0.8660254037844387076, 1.000000000000000000, 0.8660254037844387076, 1.000000000000000000, 0.8660254037844387076, 1.000000000000000000, 0.8660254037844387076, 1.000000000000000000, 0.8660254037844387076, 1.000000000000000000, 0.8660254037844387076, 1.000000000000000000, 0.8660254037844387076, 1.000000000000000000, 0.8660254037844387076, 1.000000000000000000, 0.8660254037844387076, 1.000000000000000000, 0.8660254037844387076, 1.000000000000000000, 0.8660254037844387076, 1.000000000000000000, 0.8660254037844387076, 1.000000000000000000, 0.8660254037844387076, 1.000000000000000000, 0.8660254037844387076, 1.000000000000000000, 0.8660254037844387076, 1.000000000000000000, 0.8660254037844387076, 1.000000000000000000, 0.8660254037844387076, 1.000000000000000000, 0.8660254037844387076, 1.000000000000000000, 0.8660254037844387076, 1.000000000000000000, 0.8660254037844387076, 1.000000000000000000, 0.8660254037844387076, 1.000000000000000000, 0.8660254037844387076, 1.000000000000000000, 0.8660254037844387076, 1.000000000000000000 ) ) 
 REPRESENTATION_ITEM ( '' )  );
#25069 = CARTESIAN_POINT ( 'NONE',  ( 20.64316235839397962, 17.98696498043453573, 12.25316411605952283 ) ) ;
#25070 = CARTESIAN_POINT ( 'NONE',  ( 23.67481891673307715, 18.01796466724061929, 6.690598923241489970 ) ) ;
#25071 = EDGE_LOOP ( 'NONE', ( #12031, #615, #10721, #10993 ) ) ;
#25072 = CARTESIAN_POINT ( 'NONE',  ( 4.000000000000001776, 26.70624999877097139, 11.30940107675849760 ) ) ;
#25073 = CARTESIAN_POINT ( 'NONE',  ( -1.999999999999995781, 27.79374999877096997, 5.535898384862237620 ) ) ;
#25074 = CARTESIAN_POINT ( 'NONE',  ( -4.000000000000003553, -25.00000000000000000, 8.999999999999992895 ) ) ;
#25076 = EDGE_LOOP ( 'NONE', ( #12036, #12329, #24887, #18289 ) ) ;
#25075 = CARTESIAN_POINT ( 'NONE',  ( -1.999999999999995781, 25.54374999877096997, 5.535898384862237620 ) ) ;
#25077 = CARTESIAN_POINT ( 'NONE',  ( 3.756430356250003211, 25.29062499938548569, 6.831223922626973533 ) ) ;
#25078 = CIRCLE ( 'NONE', #31, 0.5000000000000000000 ) ;
#25079 = EDGE_CURVE ( 'NONE', #8492, #8072, #5112, .T. ) ;
#25080 = ORIENTED_EDGE ( 'NONE', *, *, #15873, .F. ) ;
#25081 = CARTESIAN_POINT ( 'NONE',  ( 3.756430356249995661, -28.47812499938548569, 6.831223922626973533 ) ) ;
#25082 = ORIENTED_EDGE ( 'NONE', *, *, #9962, .F. ) ;
#25083 = EDGE_LOOP ( 'NONE', ( #14755, #2373, #6446, #8673 ) ) ;
#25084 = CARTESIAN_POINT ( 'NONE',  ( 20.28273967276687628, 22.10586454194350736, 12.79562863665509553 ) ) ;
#25085 = CARTESIAN_POINT ( 'NONE',  ( -1.878215178124996498, 27.20312499938549067, 5.746835883940462963 ) ) ;
#25086 = ADVANCED_FACE ( 'NONE', ( #14214 ), #16307, .T. ) ;
#25087 = CIRCLE ( 'NONE', #2531, 31.10000000000000142 ) ;
#25088 = CARTESIAN_POINT ( 'NONE',  ( -3.756430356249996105, -6.831223922626973533, 0.3281249993854827851 ) ) ;
#25089 = AXIS2_PLACEMENT_3D ( 'NONE', #6406, #149, #7985 ) ;
#25090 = VECTOR ( 'NONE', #686, 1000.000000000000000 ) ;
#25091 = CARTESIAN_POINT ( 'NONE',  ( 2.672651547586948120E-15, -13.33755215474602984, 4.190624999385483385 ) ) ;
#25092 = CARTESIAN_POINT ( 'NONE',  ( 11.91206721063039886, 28.72825533807133169, 1.000000000000000000 ) ) ;
#25093 = VECTOR ( 'NONE', #22753, 1000.000000000000000 ) ;
#25094 = CARTESIAN_POINT ( 'NONE',  ( -1.057460391440397258E-14, 29.10624999877096641, 4.999999999999992006 ) ) ;
#25095 = UNCERTAINTY_MEASURE_WITH_UNIT (LENGTH_MEASURE( 1.000000000000000082E-05 ), #6131, 'distance_accuracy_value', 'NONE');
#25096 = CARTESIAN_POINT ( 'NONE',  ( -3.756430356249996105, 29.37812499938548427, 6.831223922626973533 ) ) ;
#25097 = CYLINDRICAL_SURFACE ( 'NONE', #7970, 4.000000000000000000 ) ;
#25098 = CARTESIAN_POINT ( 'NONE',  ( 23.01025686871630782, -20.92219106202058754, -2.750000000000000000 ) ) ;
#25099 = CARTESIAN_POINT ( 'NONE',  ( -19.32388608118395013, 23.96296185032730364, 1.000000000000000000 ) ) ;
#25100 = CARTESIAN_POINT ( 'NONE',  ( -1.071796769724495668, -27.55134618820330061, 12.99999999999999112 ) ) ;
#25101 = CARTESIAN_POINT ( 'NONE',  ( -3.735045420075836212E-15, -28.96562499938548640, 4.662447845253954171 ) ) ;
#25102 = CARTESIAN_POINT ( 'NONE',  ( 1.878215178125000939, 26.07812499938548356, 12.25316411605952283 ) ) ;
#25103 = CARTESIAN_POINT ( 'NONE',  ( 4.000000000000001776, 27.60624999877096641, 11.30940107675849760 ) ) ;
#25104 = DIRECTION ( 'NONE',  ( 0.000000000000000000, 0.000000000000000000, 1.000000000000000000 ) ) ;
#25105 = CARTESIAN_POINT ( 'NONE',  ( -19.43607991388954304, 24.27856662945528399, -2.750000000000000000 ) ) ;
#25106 = VERTEX_POINT ( 'NONE', #6099 ) ;
#25107 = CARTESIAN_POINT ( 'NONE',  ( -28.14012133169306296, 13.24173596767408867, 1.000000000000000000 ) ) ;
#25109 = VERTEX_POINT ( 'NONE', #24276 ) ;
#25108 = CARTESIAN_POINT ( 'NONE',  ( -3.526711513754876570, 31.50000000000000000, 4.645898033750338385 ) ) ;
#25111 = ORIENTED_EDGE ( 'NONE', *, *, #8199, .T. ) ;
#25110 = EDGE_CURVE ( 'NONE', #7791, #10324, #21397, .T. ) ;
#25112 = VERTEX_POINT ( 'NONE', #8460 ) ;
#25113 = VERTEX_POINT ( 'NONE', #22439 ) ;
#25114 = VERTEX_POINT ( 'NONE', #20470 ) ;
#25115 = DIRECTION ( 'NONE',  ( 1.000000000000000000, 0.000000000000000000, 0.000000000000000000 ) ) ;
#25116 =( BOUNDED_CURVE ( )  B_SPLINE_CURVE ( 2, ( #23147, #5610, #1049, #13591, #7053, #15041, #3138, #5226, #13206 ),
 .UNSPECIFIED., .F., .F. ) 
 B_SPLINE_CURVE_WITH_KNOTS ( ( 3, 2, 2, 2, 3 ),
 ( 0.1250000000000000000, 0.1333333333333333315, 0.1499999999999999944, 0.1666666666666666574, 0.1749999999999999889 ),
 .UNSPECIFIED. ) 
 CURVE ( )  GEOMETRIC_REPRESENTATION_ITEM ( )  RATIONAL_B_SPLINE_CURVE ( ( 0.9330127018922194093, 0.9330127018922194093, 1.000000000000000000, 0.8660254037844387076, 1.000000000000000000, 0.8660254037844387076, 1.000000000000000000, 0.9330127018922194093, 0.9330127018922194093 ) ) 
 REPRESENTATION_ITEM ( '' )  );
#25117 = FACE_OUTER_BOUND ( 'NONE', #4585, .T. ) ;
#25118 = EDGE_CURVE ( 'NONE', #17279, #20930, #8442, .T. ) ;
#25119 = EDGE_CURVE ( 'NONE', #13240, #9674, #5182, .T. ) ;
#25120 = CARTESIAN_POINT ( 'NONE',  ( 4.006172263299091013E-15, 25.47812499938548925, 13.33755215474602984 ) ) ;
#25121 =( BOUNDED_CURVE ( )  B_SPLINE_CURVE ( 2, ( #7572, #3639, #2072, #3521, #17509, #13709, #10040, #7702, #9526 ),
 .UNSPECIFIED., .F., .F. ) 
 B_SPLINE_CURVE_WITH_KNOTS ( ( 3, 2, 2, 2, 3 ),
 ( 0.7750000000000000222, 0.7833333333333333259, 0.8000000000000000444, 0.8166666666666666519, 0.8250000000000000666 ),
 .UNSPECIFIED. ) 
 CURVE ( )  GEOMETRIC_REPRESENTATION_ITEM ( )  RATIONAL_B_SPLINE_CURVE ( ( 0.9330127018922194093, 0.9330127018922194093, 1.000000000000000000, 0.8660254037844387076, 1.000000000000000000, 0.8660254037844387076, 1.000000000000000000, 0.9330127018922189652, 0.9330127018922194093 ) ) 
 REPRESENTATION_ITEM ( '' )  );
#25122 = CARTESIAN_POINT ( 'NONE',  ( -3.756430356249997882, -11.16877607737301226, 4.565624999385485161 ) ) ;
#25123 = CARTESIAN_POINT ( 'NONE',  ( 2.000000000000003997, -5.535898384862238508, 2.268749998770969167 ) ) ;
#25124 = CARTESIAN_POINT ( 'NONE',  ( 19.20672417798141041, 21.86292155594071218, 12.25316411605951927 ) ) ;
#25125 = EDGE_CURVE ( 'NONE', #21178, #6707, #106, .T. ) ;
#25126 = AXIS2_PLACEMENT_3D ( 'NONE', #6120, #4157, #15945 ) ;
#25127 = CARTESIAN_POINT ( 'NONE',  ( -3.756430356249996994, 26.37812499938548783, 8.999999999999992895 ) ) ;
#25128 = VECTOR ( 'NONE', #24606, 1000.000000000000000 ) ;
#25129 = DIRECTION ( 'NONE',  ( 0.000000000000000000, -0.000000000000000000, 1.000000000000000000 ) ) ;
#25130 = CARTESIAN_POINT ( 'NONE',  ( 27.25313774936409317, -14.98253926456347074, -6.500000000000000000 ) ) ;
#25131 = CARTESIAN_POINT ( 'NONE',  ( 3.752267015613588906E-15, -4.381197846482986158, 0.1124999999999989342 ) ) ;
#25132 = DIRECTION ( 'NONE',  ( 0.8443279255020205154, 0.5358267949789882190, 0.000000000000000000 ) ) ;
#25133 = CARTESIAN_POINT ( 'NONE',  ( -30.85476721088022600, 3.897863563850190616, -6.500000000000000000 ) ) ;
#25134 = DIRECTION ( 'NONE',  ( 0.000000000000000000, 0.000000000000000000, 1.000000000000000000 ) ) ;
#25135 = CARTESIAN_POINT ( 'NONE',  ( 3.999999999999996003, -25.58124999877097139, 6.690598923241487306 ) ) ;
#25136 = AXIS2_PLACEMENT_3D ( 'NONE', #19580, #1684, #9660 ) ;
#25137 = DIRECTION ( 'NONE',  ( 1.000000000000000000, 0.000000000000000000, 0.000000000000000000 ) ) ;
#25138 = DIRECTION ( 'NONE',  ( 0.000000000000000000, -0.000000000000000000, -1.000000000000000000 ) ) ;
#25139 = VERTEX_POINT ( 'NONE', #21123 ) ;
#25140 = EDGE_CURVE ( 'NONE', #7323, #7998, #5940, .T. ) ;
#25141 = CARTESIAN_POINT ( 'NONE',  ( -3.999999999999996447, -8.999999999999992895, 8.000000000000000000 ) ) ;
#25142 = ORIENTED_EDGE ( 'NONE', *, *, #8912, .F. ) ;
#25143 = ORIENTED_EDGE ( 'NONE', *, *, #2268, .T. ) ;
#25144 = CARTESIAN_POINT ( 'NONE',  ( 17.67766952966372429, 17.67766952966365324, 4.999999999999992006 ) ) ;
#25145 = ORIENTED_EDGE ( 'NONE', *, *, #10822, .F. ) ;
#25146 = CARTESIAN_POINT ( 'NONE',  ( 3.756430356249996994, -26.82812499938548711, 8.999999999999992895 ) ) ;
#25147 = ORIENTED_EDGE ( 'NONE', *, *, #11775, .F. ) ;
#25148 = LINE ( 'NONE', #17693, #7596 ) ;
#25149 = VECTOR ( 'NONE', #25509, 1000.000000000000000 ) ;
#25150 = AXIS2_PLACEMENT_3D ( 'NONE', #7047, #3380, #19337 ) ;
#25151 = ADVANCED_FACE ( 'NONE', ( #17076 ), #8702, .T. ) ;
#25152 = VERTEX_POINT ( 'NONE', #3085 ) ;
#25153 = APPLICATION_CONTEXT ( 'automotive_design' ) ;
#25154 = CIRCLE ( 'NONE', #13874, 31.10000000000000142 ) ;
#25155 = CARTESIAN_POINT ( 'NONE',  ( 3.999999999999995559, -29.23750000000000071, 6.690598923241487306 ) ) ;
#25156 = EDGE_CURVE ( 'NONE', #20504, #8259, #15784, .T. ) ;
#25157 = CARTESIAN_POINT ( 'NONE',  ( 4.000000000000001776, 27.21250000000000213, 11.30940107675849760 ) ) ;
#25158 = CYLINDRICAL_SURFACE ( 'NONE', #21012, 4.000000000000000000 ) ;
#25159 = AXIS2_PLACEMENT_3D ( 'NONE', #20863, #15248, #9089 ) ;
#25160 = CARTESIAN_POINT ( 'NONE',  ( 17.08421000182777760, 25.98730014090436313, -2.750000000000000000 ) ) ;
#25161 = CARTESIAN_POINT ( 'NONE',  ( -25.98730014090454432, -17.08421000182750760, -2.750000000000000000 ) ) ;
#25162 = CARTESIAN_POINT ( 'NONE',  ( 17.69528343319515784, 20.35148081115446317, 12.25316411605951927 ) ) ;
#25163 = EDGE_CURVE ( 'NONE', #13512, #8734, #21133, .T. ) ;
#25164 = DIRECTION ( 'NONE',  ( 0.000000000000000000, 1.000000000000000000, 0.000000000000000000 ) ) ;
#25165 = AXIS2_PLACEMENT_3D ( 'NONE', #4586, #12566, #19475 ) ;
#25166 = CARTESIAN_POINT ( 'NONE',  ( -3.756430356249997882, 29.45312499938548356, 11.16877607737301226 ) ) ;
#25167 = AXIS2_PLACEMENT_3D ( 'NONE', #2486, #18195, #12299 ) ;
#25168 = CARTESIAN_POINT ( 'NONE',  ( 16.34066823992097994, 21.65306299583965455, 11.16877607737301048 ) ) ;
#25169 = DIRECTION ( 'NONE',  ( 0.000000000000000000, -1.000000000000000000, 0.000000000000000000 ) ) ;
#25170 = EDGE_CURVE ( 'NONE', #20504, #6543, #12464, .T. ) ;
#25171 = ORIENTED_EDGE ( 'NONE', *, *, #12872, .F. ) ;
#25172 = EDGE_LOOP ( 'NONE', ( #9155, #4790, #12125, #21728 ) ) ;
#25173 = CARTESIAN_POINT ( 'NONE',  ( -1.999999999999994893, 26.89374999877097849, 5.535898384862237620 ) ) ;
#25174 = CARTESIAN_POINT ( 'NONE',  ( 3.756430356249997438, -29.00312499938548072, 11.16877607737301048 ) ) ;
#25175 = ORIENTED_EDGE ( 'NONE', *, *, #6913, .T. ) ;
#25176 = DIRECTION ( 'NONE',  ( 1.000000000000000000, 0.000000000000000000, 0.000000000000000000 ) ) ;
#25177 = CARTESIAN_POINT ( 'NONE',  ( -1.878215178124998497, 26.90312499938548285, 12.25316411605951927 ) ) ;
#25178 = LINE ( 'NONE', #6734, #22973 ) ;
#25179 = VERTEX_POINT ( 'NONE', #20437 ) ;
#25180 = EDGE_LOOP ( 'NONE', ( #14586, #8914, #7565, #3016 ) ) ;
#25181 = DIRECTION ( 'NONE',  ( 0.000000000000000000, -1.000000000000000000, 0.000000000000000000 ) ) ;
#25182 = CIRCLE ( 'NONE', #4282, 31.10000000000000142 ) ;
#25183 = DIRECTION ( 'NONE',  ( -1.000000000000000000, 0.000000000000000000, 0.000000000000000000 ) ) ;
#25184 = VERTEX_POINT ( 'NONE', #10359 ) ;
#25185 = CARTESIAN_POINT ( 'NONE',  ( -3.756430356250002323, -29.71562499938548640, 11.16877607737301403 ) ) ;
#25186 = CYLINDRICAL_SURFACE ( 'NONE', #7196, 0.5000000000000004441 ) ;
#25187 = CARTESIAN_POINT ( 'NONE',  ( 3.756430356250002323, 26.45312499938549067, 11.16877607737301403 ) ) ;
#25188 = AXIS2_PLACEMENT_3D ( 'NONE', #23528, #21827, #25620 ) ;
#25189 = CARTESIAN_POINT ( 'NONE',  ( 3.756430356250003655, 25.25312499938548427, 8.999999999999992895 ) ) ;
#25190 = CARTESIAN_POINT ( 'NONE',  ( 3.756430356250003211, 28.74062499938548498, 8.999999999999992895 ) ) ;
#25191 = ADVANCED_FACE ( 'NONE', ( #14324 ), #10504, .F. ) ;
#25192 = ADVANCED_FACE ( 'NONE', ( #19917 ), #6581, .T. ) ;
#25193 = AXIS2_PLACEMENT_3D ( 'NONE', #3266, #13724, #23278 ) ;
#25194 = DIRECTION ( 'NONE',  ( 0.000000000000000000, -1.000000000000000000, 0.000000000000000000 ) ) ;
#25195 = APPLICATION_PROTOCOL_DEFINITION ( 'draft international standard', 'automotive_design', 1998, #15450 ) ;
#25196 = CARTESIAN_POINT ( 'NONE',  ( 0.000000000000000000, 0.000000000000000000, -6.500000000000000000 ) ) ;
#25197 = EDGE_CURVE ( 'NONE', #23824, #16937, #2193, .T. ) ;
#25198 = LINE ( 'NONE', #7278, #9651 ) ;
#25199 = CIRCLE ( 'NONE', #565, 31.10000000000000142 ) ;
#25200 = EDGE_CURVE ( 'NONE', #9659, #11524, #18123, .T. ) ;
#25201 = CARTESIAN_POINT ( 'NONE',  ( 3.735045420075836212E-15, 26.60312499938547859, 4.662447845253954171 ) ) ;
#25202 = FACE_BOUND ( 'NONE', #3147, .T. ) ;
#25203 = CARTESIAN_POINT ( 'NONE',  ( 19.78131220369370169, 16.95288507894744257, 5.535898384862238508 ) ) ;
#25204 = CARTESIAN_POINT ( 'NONE',  ( 18.25440349763447756, 18.25440349763440295, 4.662447845253954171 ) ) ;
#25205 = CARTESIAN_POINT ( 'NONE',  ( 16.24135887950949808, 21.89821312900181027, 8.999999999999992895 ) ) ;
#25206 = CARTESIAN_POINT ( 'NONE',  ( 3.735045420075836212E-15, 27.95312499938548001, 4.662447845253954171 ) ) ;
#25207 = DIRECTION ( 'NONE',  ( -0.000000000000000000, -0.000000000000000000, -1.000000000000000000 ) ) ;
#25208 = CARTESIAN_POINT ( 'NONE',  ( 22.68720666332504265, 17.37481190740622239, 6.831223922626973533 ) ) ;
#25209 = CARTESIAN_POINT ( 'NONE',  ( 2.620986760973688460E-15, -13.61880215351699874, 3.037499999999998757 ) ) ;
#25210 = ORIENTED_EDGE ( 'NONE', *, *, #20422, .F. ) ;
#25211 = CARTESIAN_POINT ( 'NONE',  ( -3.756430356249997882, 26.41562499938548569, 11.16877607737301226 ) ) ;
#25212 = CARTESIAN_POINT ( 'NONE',  ( -1.878215178125000939, -28.21562499938548640, 12.25316411605952283 ) ) ;
#25214 = ORIENTED_EDGE ( 'NONE', *, *, #16474, .F. ) ;
#25213 = DIRECTION ( 'NONE',  ( 0.000000000000000000, 0.000000000000000000, 1.000000000000000000 ) ) ;
#25215 = CARTESIAN_POINT ( 'NONE',  ( 3.756430356250003211, 26.64062499938548356, 6.831223922626973533 ) ) ;
#25216 = ORIENTED_EDGE ( 'NONE', *, *, #16798, .F. ) ;
#25217 = CARTESIAN_POINT ( 'NONE',  ( 3.756430356249997882, -28.10312499938548569, 11.16877607737301226 ) ) ;
#25218 = ORIENTED_EDGE ( 'NONE', *, *, #8266, .T. ) ;
#25219 = ORIENTED_EDGE ( 'NONE', *, *, #4335, .T. ) ;
#25220 = FILL_AREA_STYLE ('',( #1418 ) ) ;
#25221 = CARTESIAN_POINT ( 'NONE',  ( -1.878215178124996498, 28.55312499938548854, 5.746835883940462963 ) ) ;
#25222 = AXIS2_PLACEMENT_3D ( 'NONE', #7104, #10751, #14951 ) ;
#25223 = CARTESIAN_POINT ( 'NONE',  ( 3.756430356250002323, -11.16877607737301403, 1.903124999385483740 ) ) ;
#25224 = EDGE_CURVE ( 'NONE', #10602, #15596, #5535, .T. ) ;
#25225 = CARTESIAN_POINT ( 'NONE',  ( -3.756430356249995661, -6.831223922626973533, 3.590624999385483740 ) ) ;
#25226 = CARTESIAN_POINT ( 'NONE',  ( -0.5000000000000001110, 10.00000000000000000, 13.00000000000000178 ) ) ;
#25227 = DIRECTION ( 'NONE',  ( 0.000000000000000000, -0.000000000000000000, -1.000000000000000000 ) ) ;
#25228 = DIRECTION ( 'NONE',  ( 0.000000000000000000, 0.000000000000000000, 1.000000000000000000 ) ) ;
#25229 =( BOUNDED_CURVE ( )  B_SPLINE_CURVE ( 2, ( #13313, #5597, #25340, #9122, #21541, #25088, #11475, #1670, #17489, #19065, #21045, #7418, #9643, #15400, #23376, #9508, #5461, #1283, #3623, #1148, #19567, #11085, #17626, #11593, #21286, #7550, #17114, #13576, #15021, #23000, #15542, #3367, #17254, #5086, #19447, #15162, #7304, #23132, #13455, #19328, #3505, #5213, #13190, #21160, #11206, #19186, #9267, #25223, #23246, #5329, #11345, #1420, #2191, #6100, #7805, #15668, #7936, #103, #8198, #18153, #15923, #13691, #8076, #25849, #20087, #11976, #4275, #14217, #18016, #5712, #23635, #12113, #21806, #6224, #1808, #11860, #3889, #10152, #14083, #15783, #21667, #3752, #23896, #20216, #5979, #9775, #19708, #4134, #11730, #16055, #227, #16173, #24138, #24019, #22190, #17751, #12247, #2315, #19949, #25724, #23755, #10270, #22048, #25600, #5844, #7683, #13961, #2055, #13828, #1929, #19828, #9892, #17878, #21930, #4010, #10019, #24661, #12641, #350, #6608, #12374 ),
 .UNSPECIFIED., .F., .T. ) 
 B_SPLINE_CURVE_WITH_KNOTS ( ( 3, 2, 2, 2, 2, 2, 2, 2, 2, 2, 2, 2, 2, 2, 2, 2, 2, 2, 2, 2, 2, 2, 2, 2, 2, 2, 2, 2, 2, 2, 2, 2, 2, 2, 2, 2, 2, 2, 2, 2, 2, 2, 2, 2, 2, 2, 2, 2, 2, 2, 2, 2, 2, 2, 2, 2, 2, 2, 2, 2, 3 ),
 ( 0.000000000000000000, 0.01666666666666666644, 0.03333333333333333287, 0.05000000000000000278, 0.06666666666666666574, 0.08333333333333332871, 0.1000000000000000056, 0.1166666666666666685, 0.1333333333333333315, 0.1499999999999999944, 0.1666666666666666574, 0.1833333333333333204, 0.2000000000000000111, 0.2166666666666666741, 0.2333333333333333370, 0.2500000000000000000, 0.2666666666666666630, 0.2833333333333333259, 0.2999999999999999889, 0.3166666666666666519, 0.3333333333333333148, 0.3499999999999999778, 0.3666666666666666408, 0.3833333333333333592, 0.4000000000000000222, 0.4166666666666666852, 0.4333333333333333481, 0.4500000000000000111, 0.4666666666666666741, 0.4833333333333333370, 0.5000000000000000000, 0.5166666666666667185, 0.5333333333333333259, 0.5500000000000000444, 0.5666666666666666519, 0.5833333333333333703, 0.5999999999999999778, 0.6166666666666666963, 0.6333333333333333037, 0.6500000000000000222, 0.6666666666666666297, 0.6833333333333333481, 0.6999999999999999556, 0.7166666666666666741, 0.7333333333333332815, 0.7500000000000000000, 0.7666666666666667185, 0.7833333333333333259, 0.8000000000000000444, 0.8166666666666666519, 0.8333333333333333703, 0.8499999999999999778, 0.8666666666666666963, 0.8833333333333333037, 0.9000000000000000222, 0.9166666666666666297, 0.9333333333333333481, 0.9499999999999999556, 0.9666666666666666741, 0.9833333333333332815, 1.000000000000000000 ),
 .UNSPECIFIED. ) 
 CURVE ( )  GEOMETRIC_REPRESENTATION_ITEM ( )  RATIONAL_B_SPLINE_CURVE ( ( 1.000000000000000000, 0.8660254037844387076, 1.000000000000000000, 0.8660254037844387076, 1.000000000000000000, 0.8660254037844387076, 1.000000000000000000, 0.8660254037844387076, 1.000000000000000000, 0.8660254037844387076, 1.000000000000000000, 0.8660254037844387076, 1.000000000000000000, 0.8660254037844387076, 1.000000000000000000, 0.8660254037844387076, 1.000000000000000000, 0.8660254037844387076, 1.000000000000000000, 0.8660254037844387076, 1.000000000000000000, 0.8660254037844387076, 1.000000000000000000, 0.8660254037844387076, 1.000000000000000000, 0.8660254037844387076, 1.000000000000000000, 0.8660254037844387076, 1.000000000000000000, 0.8660254037844387076, 1.000000000000000000, 0.8660254037844387076, 1.000000000000000000, 0.8660254037844387076, 1.000000000000000000, 0.8660254037844387076, 1.000000000000000000, 0.8660254037844387076, 1.000000000000000000, 0.8660254037844387076, 1.000000000000000000, 0.8660254037844387076, 1.000000000000000000, 0.8660254037844387076, 1.000000000000000000, 0.8660254037844387076, 1.000000000000000000, 0.8660254037844387076, 1.000000000000000000, 0.8660254037844387076, 1.000000000000000000, 0.8660254037844387076, 1.000000000000000000, 0.8660254037844387076, 1.000000000000000000, 0.8660254037844387076, 1.000000000000000000, 0.8660254037844387076, 1.000000000000000000, 0.8660254037844387076, 1.000000000000000000, 0.8660254037844387076, 1.000000000000000000, 0.8660254037844387076, 1.000000000000000000, 0.8660254037844387076, 1.000000000000000000, 0.8660254037844387076, 1.000000000000000000, 0.8660254037844387076, 1.000000000000000000, 0.8660254037844387076, 1.000000000000000000, 0.8660254037844387076, 1.000000000000000000, 0.8660254037844387076, 1.000000000000000000, 0.8660254037844387076, 1.000000000000000000, 0.8660254037844387076, 1.000000000000000000, 0.8660254037844387076, 1.000000000000000000, 0.8660254037844387076, 1.000000000000000000, 0.8660254037844387076, 1.000000000000000000, 0.8660254037844387076, 1.000000000000000000, 0.8660254037844387076, 1.000000000000000000, 0.8660254037844387076, 1.000000000000000000, 0.8660254037844387076, 1.000000000000000000, 0.8660254037844387076, 1.000000000000000000, 0.8660254037844387076, 1.000000000000000000, 0.8660254037844387076, 1.000000000000000000, 0.8660254037844387076, 1.000000000000000000, 0.8660254037844387076, 1.000000000000000000, 0.8660254037844387076, 1.000000000000000000, 0.8660254037844387076, 1.000000000000000000, 0.8660254037844387076, 1.000000000000000000, 0.8660254037844387076, 1.000000000000000000, 0.8660254037844387076, 1.000000000000000000, 0.8660254037844387076, 1.000000000000000000, 0.8660254037844387076, 1.000000000000000000, 0.8660254037844387076, 1.000000000000000000 ) ) 
 REPRESENTATION_ITEM ( '' )  );
#25230 = CYLINDRICAL_SURFACE ( 'NONE', #19931, 31.10000000000000142 ) ;
#25231 = DIRECTION ( 'NONE',  ( 0.000000000000000000, 0.000000000000000000, -1.000000000000000000 ) ) ;
#25232 = DIRECTION ( 'NONE',  ( -0.9510565162951561957, -0.3090169943749392911, 0.000000000000000000 ) ) ;
#25233 = CARTESIAN_POINT ( 'NONE',  ( -3.999999999999996447, -8.999999999999992895, 0.6187499987709670357 ) ) ;
#25234 = CARTESIAN_POINT ( 'NONE',  ( -3.756430356250003655, -28.40312499938548640, 8.999999999999992895 ) ) ;
#25235 = DIRECTION ( 'NONE',  ( 0.000000000000000000, 0.000000000000000000, 1.000000000000000000 ) ) ;
#25237 = ADVANCED_FACE ( 'NONE', ( #20308 ), #9986, .T. ) ;
#25236 = CYLINDRICAL_SURFACE ( 'NONE', #6200, 31.10000000000000142 ) ;
#25238 = DIRECTION ( 'NONE',  ( 0.000000000000000000, 0.000000000000000000, -1.000000000000000000 ) ) ;
#25239 = CARTESIAN_POINT ( 'NONE',  ( -16.16421332384701515, -26.25859848311253941, -6.500000000000000000 ) ) ;
#25240 = EDGE_LOOP ( 'NONE', ( #19120, #16379, #9589, #897 ) ) ;
#25241 = CARTESIAN_POINT ( 'NONE',  ( 1.878215178125003382, 29.67812499938549209, 12.25316411605952283 ) ) ;
#25242 = DIRECTION ( 'NONE',  ( 0.9921147013144794302, 0.1253332335642911299, 0.000000000000000000 ) ) ;
#25244 = EDGE_LOOP ( 'NONE', ( #9219, #2249, #3743, #10463 ) ) ;
#25243 = DIRECTION ( 'NONE',  ( 0.000000000000000000, 0.000000000000000000, 1.000000000000000000 ) ) ;
#25245 = ORIENTED_EDGE ( 'NONE', *, *, #1870, .T. ) ;
#25246 = ORIENTED_EDGE ( 'NONE', *, *, #16004, .T. ) ;
#25247 = VERTEX_POINT ( 'NONE', #22020 ) ;
#25248 = EDGE_LOOP ( 'NONE', ( #15532, #240, #20018, #16764 ) ) ;
#25249 = DIRECTION ( 'NONE',  ( 0.4817536741017131585, -0.8763066800438648052, 0.000000000000000000 ) ) ;
#25250 = DIRECTION ( 'NONE',  ( 0.000000000000000000, 0.000000000000000000, 1.000000000000000000 ) ) ;
#25251 = AXIS2_PLACEMENT_3D ( 'NONE', #14866, #10789, #18919 ) ;
#25252 = CARTESIAN_POINT ( 'NONE',  ( -3.999999999999996447, 27.96250000000000568, 11.30940107675849404 ) ) ;
#25253 = CARTESIAN_POINT ( 'NONE',  ( -1.878215178124998497, -12.25316411605951927, 0.4406249993854846614 ) ) ;
#25254 = CARTESIAN_POINT ( 'NONE',  ( 3.752267015613588906E-15, -4.381197846482986158, 1.856249998770964860 ) ) ;
#25255 = DIRECTION ( 'NONE',  ( 0.000000000000000000, -0.000000000000000000, -1.000000000000000000 ) ) ;
#25256 = CARTESIAN_POINT ( 'NONE',  ( -1.878215178124995832, 25.40312499938548640, 5.746835883940462963 ) ) ;
#25257 = DIRECTION ( 'NONE',  ( 0.000000000000000000, 0.000000000000000000, 1.000000000000000000 ) ) ;
#25258 = CARTESIAN_POINT ( 'NONE',  ( -9.296355089585909904E-15, 29.10624999877097352, 4.999999999999992006 ) ) ;
#25260 = EDGE_CURVE ( 'NONE', #8556, #2078, #5150, .T. ) ;
#25259 = CARTESIAN_POINT ( 'NONE',  ( 1.878215178125004048, -5.746835883940462963, 4.265624999385483562 ) ) ;
#25261 = DIRECTION ( 'NONE',  ( 0.000000000000000000, 0.000000000000000000, 1.000000000000000000 ) ) ;
#25262 = DIRECTION ( 'NONE',  ( 0.000000000000000000, 0.000000000000000000, 1.000000000000000000 ) ) ;
#25263 = CARTESIAN_POINT ( 'NONE',  ( 3.526711513754818395, 31.50000000000000000, 4.145898033750289535 ) ) ;
#25264 = CARTESIAN_POINT ( 'NONE',  ( -2.620986760973688460E-15, -25.73124999877096997, 13.61880215351699874 ) ) ;
#25265 = CARTESIAN_POINT ( 'NONE',  ( 7.248980000273979485, -30.24338421796786847, -2.750000000000000000 ) ) ;
#25266 = CARTESIAN_POINT ( 'NONE',  ( 0.7500000000000001110, 20.00000000000000000, 17.69999999999999929 ) ) ;
#25267 = CARTESIAN_POINT ( 'NONE',  ( 0.000000000000000000, 0.000000000000000000, -6.500000000000000000 ) ) ;
#25268 = EDGE_LOOP ( 'NONE', ( #19473, #2752, #25143, #17483 ) ) ;
#25269 = CARTESIAN_POINT ( 'NONE',  ( 0.000000000000000000, 0.000000000000000000, -6.500000000000000000 ) ) ;
#25270 = ORIENTED_EDGE ( 'NONE', *, *, #10309, .T. ) ;
#25271 = EDGE_CURVE ( 'NONE', #12169, #10041, #968, .T. ) ;
#25272 = ORIENTED_EDGE ( 'NONE', *, *, #19907, .F. ) ;
#25273 = CARTESIAN_POINT ( 'NONE',  ( 4.000000000000003553, -8.999999999999992895, 18.00000000000000000 ) ) ;
#25274 = EDGE_LOOP ( 'NONE', ( #5868, #25276, #19171, #21762 ) ) ;
#25275 = CARTESIAN_POINT ( 'NONE',  ( 3.756430356249996994, -29.07812499938548356, 8.999999999999992895 ) ) ;
#25276 = ORIENTED_EDGE ( 'NONE', *, *, #15479, .T. ) ;
#25277 = CARTESIAN_POINT ( 'NONE',  ( -1.999999999999995781, 28.75000000000000000, 5.535898384862237620 ) ) ;
#25278 =( BOUNDED_CURVE ( )  B_SPLINE_CURVE ( 2, ( #25780, #4334, #2118, #12310, #8388, #16380, #11797 ),
 .UNSPECIFIED., .F., .F. ) 
 B_SPLINE_CURVE_WITH_KNOTS ( ( 3, 2, 2, 3 ),
 ( 0.4999999999999997780, 0.5166666666666664964, 0.5333333333333329929, 0.5499999999999997113 ),
 .UNSPECIFIED. ) 
 CURVE ( )  GEOMETRIC_REPRESENTATION_ITEM ( )  RATIONAL_B_SPLINE_CURVE ( ( 1.000000000000001776, 0.8660254037844369313, 1.000000000000000000, 0.8660254037844387076, 1.000000000000000000, 0.8660254037844413721, 0.9999999999999973355 ) ) 
 REPRESENTATION_ITEM ( '' )  );
#25279 = ORIENTED_EDGE ( 'NONE', *, *, #24020, .T. ) ;
#25280 = CARTESIAN_POINT ( 'NONE',  ( 4.000000000000001776, 28.11250000000000426, 11.30940107675849760 ) ) ;
#25281 = CARTESIAN_POINT ( 'NONE',  ( -3.918623196469422698, 31.50000000000000000, 13.54361004533748236 ) ) ;
#25282 = CARTESIAN_POINT ( 'NONE',  ( -26.25859848311282363, -16.66421332384654974, -6.500000000000000000 ) ) ;
#25283 = CARTESIAN_POINT ( 'NONE',  ( -25.16042852506104666, -18.28012134629567598, -6.500000000000000000 ) ) ;
#25284 = CARTESIAN_POINT ( 'NONE',  ( 18.01575495898401513, 18.01575495898394408, 13.33755215474602984 ) ) ;
#25285 = DIRECTION ( 'NONE',  ( 1.000000000000000000, 0.000000000000000000, 0.000000000000000000 ) ) ;
#25286 = ADVANCED_FACE ( 'NONE', ( #196 ), #24109, .T. ) ;
#25287 = CARTESIAN_POINT ( 'NONE',  ( 4.000000000000001776, 25.86250000000000071, 11.30940107675849760 ) ) ;
#25288 = EDGE_CURVE ( 'NONE', #11472, #22249, #22408, .T. ) ;
#25289 = CARTESIAN_POINT ( 'NONE',  ( 18.57260154916842154, 18.57260154916834693, 4.662447845253954171 ) ) ;
#25290 = CARTESIAN_POINT ( 'NONE',  ( 0.000000000000000000, 0.000000000000000000, -6.500000000000000000 ) ) ;
#25291 = VERTEX_POINT ( 'NONE', #22929 ) ;
#25293 = EDGE_CURVE ( 'NONE', #6766, #11648, #16425, .T. ) ;
#25292 = EDGE_LOOP ( 'NONE', ( #12369, #10716, #10992, #18943 ) ) ;
#25294 = CARTESIAN_POINT ( 'NONE',  ( -4.000000000000000000, 27.86874999877096926, 8.999999999999992895 ) ) ;
#25295 = CARTESIAN_POINT ( 'NONE',  ( -28.91604871112473418, -11.44867358849319849, 1.000000000000000000 ) ) ;
#25296 = VERTEX_POINT ( 'NONE', #18744 ) ;
#25297 = CARTESIAN_POINT ( 'NONE',  ( -20.20656826142249685, 23.64116323484259752, -2.750000000000000000 ) ) ;
#25298 = AXIS2_PLACEMENT_3D ( 'NONE', #16238, #21992, #24210 ) ;
#25299 = CARTESIAN_POINT ( 'NONE',  ( -1.878215178124998497, 28.70312499938548356, 12.25316411605951927 ) ) ;
#25300 = LINE ( 'NONE', #21504, #5460 ) ;
#25301 = EDGE_CURVE ( 'NONE', #9674, #18613, #9598, .T. ) ;
#25302 = ORIENTED_EDGE ( 'NONE', *, *, #3855, .T. ) ;
#25303 = EDGE_LOOP ( 'NONE', ( #4036, #21274, #11197, #8134 ) ) ;
#25304 = FACE_OUTER_BOUND ( 'NONE', #21949, .T. ) ;
#25305 = DIRECTION ( 'NONE',  ( 1.000000000000000000, 0.000000000000000000, 0.000000000000000000 ) ) ;
#25306 = ORIENTED_EDGE ( 'NONE', *, *, #17018, .T. ) ;
#25307 = CARTESIAN_POINT ( 'NONE',  ( -29.57785765677936851, -9.610428525060582317, -6.500000000000000000 ) ) ;
#25308 = CARTESIAN_POINT ( 'NONE',  ( 0.000000000000000000, 0.000000000000000000, -6.500000000000000000 ) ) ;
#25309 = CARTESIAN_POINT ( 'NONE',  ( -1.878215178124998275, 28.59062499938548640, 12.25316411605951927 ) ) ;
#25310 = DIRECTION ( 'NONE',  ( 0.000000000000000000, 0.000000000000000000, 1.000000000000000000 ) ) ;
#25311 = CARTESIAN_POINT ( 'NONE',  ( 2.000000000000005329, 25.07500000000000284, 5.535898384862238508 ) ) ;
#25312 = CONTEXT_DEPENDENT_SHAPE_REPRESENTATION ( #20789, #18856 ) ;
#25313 = DIRECTION ( 'NONE',  ( 0.000000000000000000, 0.000000000000000000, 1.000000000000000000 ) ) ;
#25314 = CARTESIAN_POINT ( 'NONE',  ( -11.44867358849371541, -28.91604871112453168, -6.500000000000000000 ) ) ;
#25315 = CARTESIAN_POINT ( 'NONE',  ( -3.756430356249997438, 25.85312499938548569, 11.16877607737301048 ) ) ;
#25316 = PRODUCT_RELATED_PRODUCT_CATEGORY ( 'part', '', ( #7967 ) ) ;
#25317 = CARTESIAN_POINT ( 'NONE',  ( -11.91206721063060670, -28.72825533807125353, 1.000000000000000000 ) ) ;
#25318 = CARTESIAN_POINT ( 'NONE',  ( 22.66069015903055117, 17.34829540311172735, 8.999999999999992895 ) ) ;
#25319 = CARTESIAN_POINT ( 'NONE',  ( 22.44855812467459089, 17.13616336875576351, 6.831223922626973533 ) ) ;
#25320 = DIRECTION ( 'NONE',  ( -0.000000000000000000, 0.000000000000000000, 1.000000000000000000 ) ) ;
#25321 = CARTESIAN_POINT ( 'NONE',  ( 4.000000000000001776, 28.11250000000000071, 11.30940107675849760 ) ) ;
#25322 = DIRECTION ( 'NONE',  ( 0.000000000000000000, 0.000000000000000000, -1.000000000000000000 ) ) ;
#25323 = CARTESIAN_POINT ( 'NONE',  ( 20.32496430686003208, 17.66876692890059530, 12.25316411605952283 ) ) ;
#25324 = CARTESIAN_POINT ( 'NONE',  ( -3.999999999999996447, -8.999999999999992895, 3.318749998770968102 ) ) ;
#25325 = ORIENTED_EDGE ( 'NONE', *, *, #17524, .F. ) ;
#25326 = FACE_OUTER_BOUND ( 'NONE', #22798, .T. ) ;
#25327 = CARTESIAN_POINT ( 'NONE',  ( -3.756430356249996994, 25.92812499938548498, 8.999999999999992895 ) ) ;
#25328 = CARTESIAN_POINT ( 'NONE',  ( 1.999999999999995781, -25.15000000000000213, 5.535898384862237620 ) ) ;
#25329 = EDGE_CURVE ( 'NONE', #20576, #9975, #3054, .T. ) ;
#25331 = ORIENTED_EDGE ( 'NONE', *, *, #2089, .T. ) ;
#25330 = LINE ( 'NONE', #3877, #19531 ) ;
#25332 = CARTESIAN_POINT ( 'NONE',  ( 3.735045420075836212E-15, 26.26562499938548356, 4.662447845253954171 ) ) ;
#25333 = EDGE_CURVE ( 'NONE', #19280, #15184, #11659, .T. ) ;
#25334 = CARTESIAN_POINT ( 'NONE',  ( 17.18149551509901940, 19.58805710660145039, 20.00001200000000168 ) ) ;
#25335 = CARTESIAN_POINT ( 'NONE',  ( -3.735045420075836212E-15, -28.40312499938548640, 4.662447845253954171 ) ) ;
#25336 = ORIENTED_EDGE ( 'NONE', *, *, #18971, .T. ) ;
#25337 = ORIENTED_EDGE ( 'NONE', *, *, #9146, .F. ) ;
#25338 = FACE_OUTER_BOUND ( 'NONE', #13840, .T. ) ;
#25339 = CARTESIAN_POINT ( 'NONE',  ( 1.878215178125006934, 25.21562499938548996, 5.746835883940462963 ) ) ;
#25340 = CARTESIAN_POINT ( 'NONE',  ( 1.878215178125004048, -5.746835883940462963, 0.2156249993854816860 ) ) ;
#25341 = CARTESIAN_POINT ( 'NONE',  ( 3.756430356250004099, -6.831223922626973533, 4.340624999385483740 ) ) ;
#25342 = CARTESIAN_POINT ( 'NONE',  ( 1.071796769724490783, 26.70759618943234059, 12.99999999999999467 ) ) ;
#25343 = DIRECTION ( 'NONE',  ( 0.000000000000000000, 0.000000000000000000, -1.000000000000000000 ) ) ;
#25344 = DIRECTION ( 'NONE',  ( 0.000000000000000000, 0.000000000000000000, 1.000000000000000000 ) ) ;
#25345 = DIRECTION ( 'NONE',  ( 0.000000000000000000, -1.000000000000000000, 0.000000000000000000 ) ) ;
#25346 = DIRECTION ( 'NONE',  ( 0.000000000000000000, 0.000000000000000000, 1.000000000000000000 ) ) ;
#25347 = ORIENTED_EDGE ( 'NONE', *, *, #13029, .T. ) ;
#25348 = CARTESIAN_POINT ( 'NONE',  ( -3.834746474454188013E-15, -27.75624999877096855, 4.999999999999992006 ) ) ;
#25349 = CARTESIAN_POINT ( 'NONE',  ( -2.672651547586948120E-15, -29.19062499938548783, 13.33755215474602984 ) ) ;
#25350 = CARTESIAN_POINT ( 'NONE',  ( 3.735045420075836212E-15, 25.81562499938548783, 4.662447845253954171 ) ) ;
#25351 = CARTESIAN_POINT ( 'NONE',  ( -3.999999999999997335, 29.70624999877096784, 11.30940107675849404 ) ) ;
#25352 = DIRECTION ( 'NONE',  ( 0.000000000000000000, 0.000000000000000000, 1.000000000000000000 ) ) ;
#25353 = EDGE_CURVE ( 'NONE', #23031, #4358, #15338, .T. ) ;
#25354 = CARTESIAN_POINT ( 'NONE',  ( 3.470226642398214878, -29.79897209676519765, 11.00633161724385900 ) ) ;
#25355 = ORIENTED_EDGE ( 'NONE', *, *, #12800, .T. ) ;
#25356 = CARTESIAN_POINT ( 'NONE',  ( 21.21320343559646915, 21.21320343559638744, 12.99999999999999289 ) ) ;
#25357 = DIRECTION ( 'NONE',  ( 0.06279051952930848890, -0.9980267284282718920, 0.000000000000000000 ) ) ;
#25359 = VERTEX_POINT ( 'NONE', #16928 ) ;
#25358 = DIRECTION ( 'NONE',  ( 0.000000000000000000, 0.000000000000000000, 1.000000000000000000 ) ) ;
#25360 = EDGE_CURVE ( 'NONE', #7582, #822, #6821, .T. ) ;
#25361 = ORIENTED_EDGE ( 'NONE', *, *, #6132, .F. ) ;
#25362 = ORIENTED_EDGE ( 'NONE', *, *, #5958, .F. ) ;
#25363 = EDGE_LOOP ( 'NONE', ( #11502, #10944, #11530, #17612 ) ) ;
#25364 = VERTEX_POINT ( 'NONE', #12741 ) ;
#25365 = CARTESIAN_POINT ( 'NONE',  ( -21.28941499438192864, 22.67092431280617859, -6.500000000000000000 ) ) ;
#25366 = CARTESIAN_POINT ( 'NONE',  ( -1.071796769724493448, 29.12634618820329990, 4.999999999999995559 ) ) ;
#25367 = CARTESIAN_POINT ( 'NONE',  ( 1.878215178125006934, 25.21562499938548996, 5.746835883940462963 ) ) ;
#25368 = ADVANCED_FACE ( 'NONE', ( #5016 ), #2672, .F. ) ;
#25369 = CARTESIAN_POINT ( 'NONE',  ( -1.878215178124998497, -12.25316411605951927, 1.790624999385481697 ) ) ;
#25370 = CARTESIAN_POINT ( 'NONE',  ( 2.000000000000003997, -5.535898384862238508, 2.718749998770968013 ) ) ;
#25371 = DIRECTION ( 'NONE',  ( 0.000000000000000000, 0.000000000000000000, -1.000000000000000000 ) ) ;
#25372 = CARTESIAN_POINT ( 'NONE',  ( 1.878215178125004048, 28.47812499938548569, 5.746835883940462963 ) ) ;
#25373 = CARTESIAN_POINT ( 'NONE',  ( 2.000000000000000888, -12.46410161513774817, 3.918749998770967746 ) ) ;
#25374 = CARTESIAN_POINT ( 'NONE',  ( 3.469446951953614189E-15, 31.50000000000000000, 8.999999999999992895 ) ) ;
#25375 = CARTESIAN_POINT ( 'NONE',  ( 4.000000000000001776, -11.30940107675849760, 2.662499999999997424 ) ) ;
#25376 = CARTESIAN_POINT ( 'NONE',  ( -3.834746474454188013E-15, -25.95624999877096428, 4.999999999999992006 ) ) ;
#25377 = CARTESIAN_POINT ( 'NONE',  ( 4.393401135981119587, 30.78811501957143193, -6.500000000000000000 ) ) ;
#25378 = CARTESIAN_POINT ( 'NONE',  ( 25.98730014090437734, -17.08421000182775984, 1.000000000000000000 ) ) ;
#25379 = CARTESIAN_POINT ( 'NONE',  ( 3.999999999999996003, -27.38124999877096855, 6.690598923241487306 ) ) ;
#25380 = CARTESIAN_POINT ( 'NONE',  ( 3.756430356250003211, -6.831223922626973533, 4.340624999385483740 ) ) ;
#25381 = CARTESIAN_POINT ( 'NONE',  ( 0.000000000000000000, 10.00000000000000000, 17.00000000000000000 ) ) ;
#25382 = AXIS2_PLACEMENT_3D ( 'NONE', #7692, #9515, #5718 ) ;
#25383 = CARTESIAN_POINT ( 'NONE',  ( 4.000000000000003553, -8.999999999999992895, 3.093749998770968457 ) ) ;
#25384 = CARTESIAN_POINT ( 'NONE',  ( -1.071796769724487230, 25.58259618943233704, 4.999999999999992006 ) ) ;
#25385 = ORIENTED_EDGE ( 'NONE', *, *, #7002, .F. ) ;
#25386 = LINE ( 'NONE', #3426, #25044 ) ;
#25387 = ORIENTED_EDGE ( 'NONE', *, *, #1144, .T. ) ;
#25388 = ADVANCED_FACE ( 'NONE', ( #18885 ), #25158, .F. ) ;
#25389 = ORIENTED_EDGE ( 'NONE', *, *, #16029, .T. ) ;
#25390 = DIRECTION ( 'NONE',  ( 1.000000000000000000, 0.000000000000000000, 0.000000000000000000 ) ) ;
#25391 = ORIENTED_EDGE ( 'NONE', *, *, #7631, .T. ) ;
#25392 = CARTESIAN_POINT ( 'NONE',  ( -3.756430356250004099, -27.54062499938548569, 6.831223922626973533 ) ) ;
#25393 = ORIENTED_EDGE ( 'NONE', *, *, #5551, .F. ) ;
#25394 = FACE_OUTER_BOUND ( 'NONE', #14854, .T. ) ;
#25395 = EDGE_CURVE ( 'NONE', #8379, #1305, #17852, .T. ) ;
#25396 = VERTEX_POINT ( 'NONE', #5774 ) ;
#25397 = CARTESIAN_POINT ( 'NONE',  ( 4.000000000000003553, 27.73750000000000071, 6.690598923241489970 ) ) ;
#25398 = DIRECTION ( 'NONE',  ( -0.000000000000000000, -1.000000000000000000, -0.000000000000000000 ) ) ;
#25399 = EDGE_CURVE ( 'NONE', #789, #21593, #23693, .T. ) ;
#25400 = LINE ( 'NONE', #25160, #23439 ) ;
#25401 = CARTESIAN_POINT ( 'NONE',  ( 3.469446951953614189E-15, 40.00000000000000000, 8.999999999999992895 ) ) ;
#25402 = CARTESIAN_POINT ( 'NONE',  ( 19.49840572522085935, 22.15460310318015758, 5.746835883940462963 ) ) ;
#25403 = DIRECTION ( 'NONE',  ( -1.000000000000000000, 0.000000000000000000, -0.000000000000000000 ) ) ;
#25404 = AXIS2_PLACEMENT_3D ( 'NONE', #24605, #18481, #12839 ) ;
#25405 = CARTESIAN_POINT ( 'NONE',  ( -3.756430356249995661, 29.37812499938548427, 6.831223922626973533 ) ) ;
#25406 = CARTESIAN_POINT ( 'NONE',  ( 20.72271187127746828, 18.06651449331802439, 12.25316411605952283 ) ) ;
#25407 = DIRECTION ( 'NONE',  ( 1.000000000000000000, 0.000000000000000000, 0.000000000000000000 ) ) ;
#25408 = ORIENTED_EDGE ( 'NONE', *, *, #24459, .T. ) ;
#25409 = VERTEX_POINT ( 'NONE', #17432 ) ;
#25410 = CARTESIAN_POINT ( 'NONE',  ( 4.000000000000005329, 28.99374999877097281, 8.999999999999992895 ) ) ;
#25411 = CARTESIAN_POINT ( 'NONE',  ( 4.000000000000001776, 28.11250000000000071, 11.30940107675849760 ) ) ;
#25412 = ORIENTED_EDGE ( 'NONE', *, *, #6680, .F. ) ;
#25413 = CARTESIAN_POINT ( 'NONE',  ( 3.834746474454188013E-15, 25.95624999877096428, 4.999999999999992006 ) ) ;
#25414 = CIRCLE ( 'NONE', #12461, 31.10000000000000142 ) ;
#25415 = CARTESIAN_POINT ( 'NONE',  ( 3.756430356250004099, 28.89062499938548356, 6.831223922626973533 ) ) ;
#25416 = CARTESIAN_POINT ( 'NONE',  ( -3.137519842735244810E-15, 27.30624999877096926, 4.999999999999991118 ) ) ;
#25417 = ORIENTED_EDGE ( 'NONE', *, *, #2225, .F. ) ;
#25418 = ORIENTED_EDGE ( 'NONE', *, *, #21035, .F. ) ;
#25419 = AXIS2_PLACEMENT_3D ( 'NONE', #13406, #7264, #15358 ) ;
#25420 = EDGE_CURVE ( 'NONE', #25045, #5585, #24351, .T. ) ;
#25421 = CARTESIAN_POINT ( 'NONE',  ( 9.133673601486471227, 29.72853858738282185, -6.500000000000000000 ) ) ;
#25422 = AXIS2_PLACEMENT_3D ( 'NONE', #1467, #17547, #25521 ) ;
#25423 = VERTEX_POINT ( 'NONE', #19504 ) ;
#25424 = CARTESIAN_POINT ( 'NONE',  ( 0.4150711328764374874, 38.77044187147116361, 14.71462540935539920 ) ) ;
#25425 = CARTESIAN_POINT ( 'NONE',  ( -3.756430356249995661, 25.77812499938548640, 6.831223922626973533 ) ) ;
#25426 = CARTESIAN_POINT ( 'NONE',  ( 3.756430356250003211, 26.94062499938548783, 8.999999999999992895 ) ) ;
#25427 = ADVANCED_FACE ( 'NONE', ( #17562 ), #3821, .T. ) ;
#25428 = CARTESIAN_POINT ( 'NONE',  ( 1.859271017917182139E-15, 28.48749999999999716, 12.99999999999999289 ) ) ;
#25429 = CARTESIAN_POINT ( 'NONE',  ( -1.999999999999996669, 26.50000000000000355, 5.535898384862237620 ) ) ;
#25430 = AXIS2_PLACEMENT_3D ( 'NONE', #3103, #11068, #14615 ) ;
#25431 = EDGE_CURVE ( 'NONE', #22996, #7429, #21488, .T. ) ;
#25432 = CARTESIAN_POINT ( 'NONE',  ( 3.756430356250004099, 28.77812499938548285, 6.831223922626973533 ) ) ;
#25433 = CARTESIAN_POINT ( 'NONE',  ( -1.999999999999998224, 27.10000000000000142, 12.46410161513774639 ) ) ;
#25434 = VECTOR ( 'NONE', #24386, 1000.000000000000000 ) ;
#25435 = CARTESIAN_POINT ( 'NONE',  ( 26.52310962334739486, -16.23990935651726275, 1.000000000000000000 ) ) ;
#25436 = CARTESIAN_POINT ( 'NONE',  ( 3.756430356250003655, 26.94062499938548427, 8.999999999999992895 ) ) ;
#25437 = VECTOR ( 'NONE', #4574, 1000.000000000000000 ) ;
#25438 = DIRECTION ( 'NONE',  ( 0.000000000000000000, -1.000000000000000000, 0.000000000000000000 ) ) ;
#25439 = CARTESIAN_POINT ( 'NONE',  ( 22.44180146790808905, 16.78494721841563475, 6.690598923241489970 ) ) ;
#25440 = CARTESIAN_POINT ( 'NONE',  ( 17.61346044605677008, 22.92585520197544469, 11.16877607737301226 ) ) ;
#25441 = CARTESIAN_POINT ( 'NONE',  ( 17.23572779142213918, 22.89258204091444782, 8.999999999999992895 ) ) ;
#25442 = CYLINDRICAL_SURFACE ( 'NONE', #18164, 4.000000000000000000 ) ;
#25443 = CARTESIAN_POINT ( 'NONE',  ( 2.000000000000000888, -12.46410161513774817, 3.018749998770966503 ) ) ;
#25444 = CARTESIAN_POINT ( 'NONE',  ( 16.84448182151639628, 22.15687657743507089, 6.831223922626973533 ) ) ;
#25445 = AXIS2_PLACEMENT_3D ( 'NONE', #5517, #25524, #7350 ) ;
#25446 = CARTESIAN_POINT ( 'NONE',  ( 0.000000000000000000, 0.000000000000000000, 17.00000000000000000 ) ) ;
#25447 = VERTEX_POINT ( 'NONE', #9574 ) ;
#25448 = CARTESIAN_POINT ( 'NONE',  ( 19.32479908713171213, 17.80904955927959676, 12.99999999999999112 ) ) ;
#25449 = EDGE_CURVE ( 'NONE', #19514, #24761, #560, .T. ) ;
#25450 = CARTESIAN_POINT ( 'NONE',  ( 3.999999999999996003, -26.08750000000000213, 6.690598923241487306 ) ) ;
#25452 = VERTEX_POINT ( 'NONE', #25537 ) ;
#25451 = CARTESIAN_POINT ( 'NONE',  ( 1.952785157361432100, -31.03863125411925949, -6.500000000000000000 ) ) ;
#25453 = CARTESIAN_POINT ( 'NONE',  ( 3.756430356250003655, 26.60312499938548569, 8.999999999999992895 ) ) ;
#25454 = VECTOR ( 'NONE', #11175, 1000.000000000000000 ) ;
#25455 = CARTESIAN_POINT ( 'NONE',  ( -3.959305671612554781E-15, -30.00000000000000355, 12.99999999999999289 ) ) ;
#25456 = AXIS2_PLACEMENT_3D ( 'NONE', #929, #3254, #5231 ) ;
#25457 = CARTESIAN_POINT ( 'NONE',  ( 23.36965697125207342, 11.52193136556788211, 20.00001200000000523 ) ) ;
#25458 = LINE ( 'NONE', #9886, #24663 ) ;
#25459 = ORIENTED_EDGE ( 'NONE', *, *, #2241, .T. ) ;
#25460 = ORIENTED_EDGE ( 'NONE', *, *, #9072, .F. ) ;
#25461 = CARTESIAN_POINT ( 'NONE',  ( 1.878215178125001605, 25.96562499938548996, 12.25316411605952283 ) ) ;
#25462 = AXIS2_PLACEMENT_3D ( 'NONE', #16695, #14600, #2701 ) ;
#25463 = CIRCLE ( 'NONE', #14192, 0.5000000000000001110 ) ;
#25464 = CARTESIAN_POINT ( 'NONE',  ( 10.08469938919477649, -29.41953157733097868, -2.750000000000000000 ) ) ;
#25465 = EDGE_CURVE ( 'NONE', #12169, #1343, #8488, .T. ) ;
#25466 = AXIS2_PLACEMENT_3D ( 'NONE', #1052, #21311, #14916 ) ;
#25467 = CARTESIAN_POINT ( 'NONE',  ( 1.878215178125000939, -12.25316411605952283, 3.778124999385484628 ) ) ;
#25468 = PRESENTATION_STYLE_ASSIGNMENT (( #21290 ) ) ;
#25469 = EDGE_CURVE ( 'NONE', #19738, #18585, #13383, .T. ) ;
#25470 = DIRECTION ( 'NONE',  ( -0.000000000000000000, 0.000000000000000000, 1.000000000000000000 ) ) ;
#25471 = AXIS2_PLACEMENT_3D ( 'NONE', #11126, #20813, #2897 ) ;
#25472 = EDGE_CURVE ( 'NONE', #16189, #8379, #17818, .T. ) ;
#25473 = CARTESIAN_POINT ( 'NONE',  ( 23.96296185032695192, -19.82388608118436935, -6.500000000000000000 ) ) ;
#25474 = DIRECTION ( 'NONE',  ( 1.000000000000000000, 0.000000000000000000, 0.000000000000000000 ) ) ;
#25475 = CARTESIAN_POINT ( 'NONE',  ( -1.071796769724490117, 26.48259618943233562, 4.999999999999992895 ) ) ;
#25476 = CARTESIAN_POINT ( 'NONE',  ( 1.071796769724494558, 25.93615380933863435, 4.999999999999992895 ) ) ;
#25477 = DIRECTION ( 'NONE',  ( 1.000000000000000000, 0.000000000000000000, 0.000000000000000000 ) ) ;
#25478 = DIRECTION ( 'NONE',  ( -0.6845471059286831750, 0.7289686274214168815, 0.000000000000000000 ) ) ;
#25479 = ORIENTED_EDGE ( 'NONE', *, *, #15711, .F. ) ;
#25480 = CYLINDRICAL_SURFACE ( 'NONE', #6332, 30.00000000000000355 ) ;
#25481 = CARTESIAN_POINT ( 'NONE',  ( -3.756430356250004099, -28.44062499938548783, 6.831223922626973533 ) ) ;
#25482 = CARTESIAN_POINT ( 'NONE',  ( -3.756430356249997882, 27.31562499938548427, 11.16877607737301226 ) ) ;
#25483 = AXIS2_PLACEMENT_3D ( 'NONE', #11512, #7337, #19363 ) ;
#25484 = DIRECTION ( 'NONE',  ( 1.000000000000000000, 0.000000000000000000, 0.000000000000000000 ) ) ;
#25485 = DIRECTION ( 'NONE',  ( -0.000000000000000000, 1.000000000000000000, -0.000000000000000000 ) ) ;
#25486 = CARTESIAN_POINT ( 'NONE',  ( 3.118766433812622196, 38.97868814324865383, 13.55653794922876898 ) ) ;
#25487 = VERTEX_POINT ( 'NONE', #21606 ) ;
#25488 = CARTESIAN_POINT ( 'NONE',  ( 1.878215178125001605, 29.22812499938549280, 12.25316411605952283 ) ) ;
#25489 = DIRECTION ( 'NONE',  ( -0.000000000000000000, -1.000000000000000000, -0.000000000000000000 ) ) ;
#25491 = ORIENTED_EDGE ( 'NONE', *, *, #22581, .F. ) ;
#25490 = CARTESIAN_POINT ( 'NONE',  ( 3.999999999999997335, -26.55624999877096570, 11.30940107675849404 ) ) ;
#25492 = EDGE_LOOP ( 'NONE', ( #25111, #10595, #22302, #22283 ) ) ;
#25493 = VECTOR ( 'NONE', #1377, 1000.000000000000000 ) ;
#25494 = ORIENTED_EDGE ( 'NONE', *, *, #3029, .T. ) ;
#25495 = VERTEX_POINT ( 'NONE', #3683 ) ;
#25496 = ORIENTED_EDGE ( 'NONE', *, *, #539, .F. ) ;
#25497 = LINE ( 'NONE', #13604, #15145 ) ;
#25498 =( BOUNDED_CURVE ( )  B_SPLINE_CURVE ( 2, ( #1436, #3905, #11609, #5477, #21683, #15421, #15681, #17892, #23649 ),
 .UNSPECIFIED., .F., .F. ) 
 B_SPLINE_CURVE_WITH_KNOTS ( ( 3, 2, 2, 2, 3 ),
 ( 0.1750000000000000167, 0.1833333333333333204, 0.2000000000000000111, 0.2166666666666666741, 0.2250000000000000056 ),
 .UNSPECIFIED. ) 
 CURVE ( )  GEOMETRIC_REPRESENTATION_ITEM ( )  RATIONAL_B_SPLINE_CURVE ( ( 0.9330127018922194093, 0.9330127018922196314, 1.000000000000000000, 0.8660254037844387076, 1.000000000000000000, 0.8660254037844387076, 1.000000000000000000, 0.9330127018922194093, 0.9330127018922194093 ) ) 
 REPRESENTATION_ITEM ( '' )  );
#25499 = CARTESIAN_POINT ( 'NONE',  ( -1.071796769724498999, -28.00134618820329635, 12.99999999999998757 ) ) ;
#25500 = VECTOR ( 'NONE', #6249, 1000.000000000000000 ) ;
#25501 = CARTESIAN_POINT ( 'NONE',  ( 1.487416814333745711E-14, 28.03750000000001208, 12.99999999999999289 ) ) ;
#25502 = VECTOR ( 'NONE', #25227, 1000.000000000000000 ) ;
#25503 = CARTESIAN_POINT ( 'NONE',  ( 1.878215178125004048, -5.746835883940462963, 2.465624999385483740 ) ) ;
#25504 = CARTESIAN_POINT ( 'NONE',  ( 2.000000000000000888, -12.46410161513774817, 0.7687499987709678351 ) ) ;
#25505 = EDGE_CURVE ( 'NONE', #16708, #15212, #11537, .T. ) ;
#25506 = CARTESIAN_POINT ( 'NONE',  ( 2.672651547586948120E-15, 28.29062499938548569, 13.33755215474602984 ) ) ;
#25507 = EDGE_CURVE ( 'NONE', #3609, #1503, #11510, .T. ) ;
#25508 = CARTESIAN_POINT ( 'NONE',  ( -2.000000000000000888, -26.66874999877096641, 12.46410161513774817 ) ) ;
#25509 = DIRECTION ( 'NONE',  ( -0.7071067811865487940, -0.7071067811865463515, 0.000000000000000000 ) ) ;
#25510 = VECTOR ( 'NONE', #21924, 1000.000000000000000 ) ;
#25511 = CARTESIAN_POINT ( 'NONE',  ( 2.620986760973688460E-15, -13.61880215351699874, 2.137499999999999734 ) ) ;
#25512 = DIRECTION ( 'NONE',  ( 1.000000000000000000, 0.000000000000000000, 0.000000000000000000 ) ) ;
#25513 = DIRECTION ( 'NONE',  ( 0.000000000000000000, -0.000000000000000000, 1.000000000000000000 ) ) ;
#25514 = DIRECTION ( 'NONE',  ( 0.000000000000000000, 0.000000000000000000, 1.000000000000000000 ) ) ;
#25515 = CARTESIAN_POINT ( 'NONE',  ( 1.999999999999995781, -26.89374999877097139, 5.535898384862237620 ) ) ;
#25516 = ADVANCED_FACE ( 'NONE', ( #17318 ), #9716, .T. ) ;
#25517 = VECTOR ( 'NONE', #19107, 1000.000000000000000 ) ;
#25518 = CARTESIAN_POINT ( 'NONE',  ( 3.756430356250003655, 28.40312499938548640, 8.999999999999992895 ) ) ;
#25519 = CIRCLE ( 'NONE', #7132, 0.4999999999999995004 ) ;
#25520 = CARTESIAN_POINT ( 'NONE',  ( 1.487416814333745711E-14, 28.43124999877096926, 12.99999999999999289 ) ) ;
#25521 = DIRECTION ( 'NONE',  ( 1.000000000000000000, 0.000000000000000000, 0.000000000000000000 ) ) ;
#25522 = CARTESIAN_POINT ( 'NONE',  ( -1.859271017917182139E-15, -28.88124999877096499, 12.99999999999999289 ) ) ;
#25523 = ORIENTED_EDGE ( 'NONE', *, *, #1798, .F. ) ;
#25524 = DIRECTION ( 'NONE',  ( 0.000000000000000000, 0.000000000000000000, 1.000000000000000000 ) ) ;
#25525 = ORIENTED_EDGE ( 'NONE', *, *, #14100, .F. ) ;
#25526 = AXIS2_PLACEMENT_3D ( 'NONE', #17757, #17882, #1814 ) ;
#25527 = ORIENTED_EDGE ( 'NONE', *, *, #7524, .F. ) ;
#25528 = DIRECTION ( 'NONE',  ( 0.000000000000000000, 0.000000000000000000, 1.000000000000000000 ) ) ;
#25529 = ORIENTED_EDGE ( 'NONE', *, *, #4012, .T. ) ;
#25530 = B_SPLINE_CURVE_WITH_KNOTS ( 'NONE', 3,
 ( #2648, #3036, #4596, #17025, #22783, #23043, #3155, #950, #15067, #21079, #20810, #12717, #16908, #13108, #4860, #8652, #6685, #6557, #24991, #24743, #12969, #14678, #22904, #9043, #2893, #12836, #20953, #10860, #7077, #10609, #11123, #10729, #22658, #19101 ),
 .UNSPECIFIED., .F., .F.,
 ( 4, 2, 2, 2, 2, 2, 2, 2, 2, 2, 2, 2, 2, 2, 2, 2, 4 ),
 ( 0.5000000000000000000, 0.5312500000000000000, 0.5625000000000000000, 0.5937500000000000000, 0.6250000000000000000, 0.6562500000000000000, 0.6875000000000000000, 0.7187500000000000000, 0.7500000000000000000, 0.7812500000000000000, 0.8125000000000000000, 0.8437500000000000000, 0.8750000000000000000, 0.9062500000000000000, 0.9375000000000000000, 0.9687500000000000000, 1.000000000000000000 ),
 .UNSPECIFIED. ) ;
#25531 = CARTESIAN_POINT ( 'NONE',  ( -1.878215178125000939, -29.22812499938548569, 12.25316411605952283 ) ) ;
#25532 = VERTEX_POINT ( 'NONE', #11802 ) ;
#25533 = CARTESIAN_POINT ( 'NONE',  ( -3.137519842735244810E-15, 26.91249999999999787, 4.999999999999991118 ) ) ;
#25534 = VECTOR ( 'NONE', #11053, 1000.000000000000000 ) ;
#25535 = VERTEX_POINT ( 'NONE', #13519 ) ;
#25536 = CARTESIAN_POINT ( 'NONE',  ( -1.999999999999998224, 26.20000000000000284, 12.46410161513774639 ) ) ;
#25537 = CARTESIAN_POINT ( 'NONE',  ( -30.53863125411922752, 1.952785157361987878, -6.500000000000000000 ) ) ;
#25538 = AXIS2_PLACEMENT_3D ( 'NONE', #2977, #4684, #10945 ) ;
#25539 = VECTOR ( 'NONE', #6690, 1000.000000000000000 ) ;
#25540 = CARTESIAN_POINT ( 'NONE',  ( 28.91604871112457076, -11.44867358849361416, 1.000000000000000000 ) ) ;
#25541 = DIRECTION ( 'NONE',  ( 0.000000000000000000, -1.000000000000000000, 0.000000000000000000 ) ) ;
#25542 = CARTESIAN_POINT ( 'NONE',  ( 17.56042743746777646, 22.87282219338644751, 6.831223922626973533 ) ) ;
#25543 = EDGE_CURVE ( 'NONE', #8796, #12340, #5977, .T. ) ;
#25544 = DIRECTION ( 'NONE',  ( 0.000000000000000000, 0.000000000000000000, 1.000000000000000000 ) ) ;
#25545 = EDGE_CURVE ( 'NONE', #13257, #9975, #17698, .T. ) ;
#25546 = CARTESIAN_POINT ( 'NONE',  ( -3.999999999999996447, 27.47499999999999787, 8.999999999999992895 ) ) ;
#25547 = CARTESIAN_POINT ( 'NONE',  ( 2.000000000000000888, 25.82499999999999929, 12.46410161513774817 ) ) ;
#25548 = CARTESIAN_POINT ( 'NONE',  ( 4.000000000000003553, -8.999999999999992895, 3.993749998770966592 ) ) ;
#25549 = AXIS2_PLACEMENT_3D ( 'NONE', #1747, #21995, #11922 ) ;
#25550 = VERTEX_POINT ( 'NONE', #13249 ) ;
#25551 = ORIENTED_EDGE ( 'NONE', *, *, #25793, .F. ) ;
#25552 = CARTESIAN_POINT ( 'NONE',  ( -1.999999999999996669, 29.29374999877097707, 12.46410161513774639 ) ) ;
#25553 = AXIS2_PLACEMENT_3D ( 'NONE', #21528, #13439, #17477 ) ;
#25554 = AXIS2_PLACEMENT_3D ( 'NONE', #13125, #1601, #21095 ) ;
#25555 = ADVANCED_FACE ( 'NONE', ( #15609 ), #21218, .F. ) ;
#25556 = ORIENTED_EDGE ( 'NONE', *, *, #25688, .F. ) ;
#25557 = CARTESIAN_POINT ( 'NONE',  ( 3.469446951953614189E-15, 31.50000000000000000, 8.999999999999992895 ) ) ;
#25558 = CARTESIAN_POINT ( 'NONE',  ( 3.756430356250004099, 27.54062499938548569, 6.831223922626973533 ) ) ;
#25559 = DIRECTION ( 'NONE',  ( 1.000000000000000000, 0.000000000000000000, 0.000000000000000000 ) ) ;
#25560 = VERTEX_POINT ( 'NONE', #25281 ) ;
#25561 = ORIENTED_EDGE ( 'NONE', *, *, #25604, .F. ) ;
#25562 = VECTOR ( 'NONE', #18959, 1000.000000000000000 ) ;
#25563 = LINE ( 'NONE', #5423, #20486 ) ;
#25564 = VERTEX_POINT ( 'NONE', #7362 ) ;
#25565 = CARTESIAN_POINT ( 'NONE',  ( 3.041615118360314618, 38.64891868624847149, 4.001525436476169872 ) ) ;
#25566 = DIRECTION ( 'NONE',  ( 0.000000000000000000, 0.000000000000000000, 1.000000000000000000 ) ) ;
#25567 = CARTESIAN_POINT ( 'NONE',  ( -2.003086131649545506E-15, 27.27812499938548996, 13.33755215474603162 ) ) ;
#25568 = AXIS2_PLACEMENT_3D ( 'NONE', #21321, #18180, #2222 ) ;
#25569 = LINE ( 'NONE', #3856, #24278 ) ;
#25570 = CARTESIAN_POINT ( 'NONE',  ( -3.999999999999996447, 26.57500000000000639, 8.999999999999992895 ) ) ;
#25571 = CARTESIAN_POINT ( 'NONE',  ( 3.756430356250003655, 28.74062499938548498, 8.999999999999992895 ) ) ;
#25572 = CARTESIAN_POINT ( 'NONE',  ( 3.469446951953614189E-15, 35.50000000000000711, 8.999999999999992895 ) ) ;
#25573 = CARTESIAN_POINT ( 'NONE',  ( 3.999999999999997335, -28.80624999877096926, 11.30940107675849404 ) ) ;
#25574 = CARTESIAN_POINT ( 'NONE',  ( 3.756430356250002323, 28.70312499938548356, 11.16877607737301403 ) ) ;
#25575 = EDGE_CURVE ( 'NONE', #12924, #8943, #10660, .T. ) ;
#25576 = CARTESIAN_POINT ( 'NONE',  ( -2.007320019195686811, -29.93357098804190741, 5.530155478426868498 ) ) ;
#25577 = CARTESIAN_POINT ( 'NONE',  ( 20.41770830676159676, 17.58928118201533408, 5.535898384862238508 ) ) ;
#25578 = CARTESIAN_POINT ( 'NONE',  ( 21.78337204305729458, 19.12717466509784003, 5.746835883940462963 ) ) ;
#25579 = DIRECTION ( 'NONE',  ( 0.000000000000000000, 0.000000000000000000, -1.000000000000000000 ) ) ;
#25580 = CARTESIAN_POINT ( 'NONE',  ( 1.859271017917182139E-15, 29.33124999877096428, 12.99999999999999289 ) ) ;
#25581 = CARTESIAN_POINT ( 'NONE',  ( 1.071796769724489895, 27.10134618820330843, 12.99999999999999467 ) ) ;
#25582 = COLOUR_RGB ( '',0.8941176470588234615, 0.8941176470588234615, 0.8941176470588234615 ) ;
#25583 = CARTESIAN_POINT ( 'NONE',  ( 17.79907597611823533, 23.11147073203690994, 6.831223922626973533 ) ) ;
#25584 = CARTESIAN_POINT ( 'NONE',  ( 0.000000000000000000, 0.000000000000000000, 1.000000000000000000 ) ) ;
#25585 = VERTEX_POINT ( 'NONE', #16512 ) ;
#25586 = CARTESIAN_POINT ( 'NONE',  ( 4.000000000000003553, 25.88124999877096499, 6.690598923241489970 ) ) ;
#25587 = CARTESIAN_POINT ( 'NONE',  ( 1.999999999999998224, -26.20000000000000284, 12.46410161513774639 ) ) ;
#25589 = ORIENTED_EDGE ( 'NONE', *, *, #21913, .F. ) ;
#25588 = CARTESIAN_POINT ( 'NONE',  ( -3.756430356249996549, 25.96562499938548996, 11.16877607737301048 ) ) ;
#25590 = ADVANCED_FACE ( 'NONE', ( #14926 ), #22897, .T. ) ;
#25591 = CARTESIAN_POINT ( 'NONE',  ( -1.878215178124998497, 29.15312499938548640, 12.25316411605951927 ) ) ;
#25592 = CIRCLE ( 'NONE', #8476, 2.899999999999999911 ) ;
#25593 = DIRECTION ( 'NONE',  ( 0.000000000000000000, 0.000000000000000000, 1.000000000000000000 ) ) ;
#25594 = CARTESIAN_POINT ( 'NONE',  ( 26.00000000000000355, 1.592040838891558898E-15, 20.00000599999999906 ) ) ;
#25595 = LINE ( 'NONE', #25844, #6706 ) ;
#25596 = ORIENTED_EDGE ( 'NONE', *, *, #10988, .F. ) ;
#25597 = ORIENTED_EDGE ( 'NONE', *, *, #19247, .T. ) ;
#25598 = CARTESIAN_POINT ( 'NONE',  ( 6.009258394948636914E-15, 26.15312499938548640, 4.662447845253954171 ) ) ;
#25599 = AXIS2_PLACEMENT_3D ( 'NONE', #1481, #9835, #9452 ) ;
#25600 = CARTESIAN_POINT ( 'NONE',  ( -3.756430356249997438, -11.16877607737301048, 4.003124999385478056 ) ) ;
#25601 = VECTOR ( 'NONE', #15886, 1000.000000000000000 ) ;
#25602 = LINE ( 'NONE', #8078, #16283 ) ;
#25603 =( NAMED_UNIT ( * ) SI_UNIT ( $, .STERADIAN. ) SOLID_ANGLE_UNIT ( ) );
#25604 = EDGE_CURVE ( 'NONE', #24827, #13859, #20592, .T. ) ;
#25605 = CARTESIAN_POINT ( 'NONE',  ( -26.50000000000000355, 0.5000000000000000000, 19.50000000000000000 ) ) ;
#25606 = CARTESIAN_POINT ( 'NONE',  ( 2.000000000000000000, 26.72500000000000497, 12.46410161513774817 ) ) ;
#25607 = LINE ( 'NONE', #15284, #24281 ) ;
#25608 = DIRECTION ( 'NONE',  ( -0.000000000000000000, -0.000000000000000000, -1.000000000000000000 ) ) ;
#25609 = CARTESIAN_POINT ( 'NONE',  ( 20.20656826142266738, -23.64116323484245541, -2.750000000000000000 ) ) ;
#25610 = DIRECTION ( 'NONE',  ( -1.000000000000000000, 0.000000000000000000, 0.000000000000000000 ) ) ;
#25611 = CARTESIAN_POINT ( 'NONE',  ( 18.99023649137220104, 18.99023649137212288, 4.381197846482986158 ) ) ;
#25612 = ORIENTED_EDGE ( 'NONE', *, *, #24459, .F. ) ;
#25613 = FACE_OUTER_BOUND ( 'NONE', #11190, .T. ) ;
#25614 = CARTESIAN_POINT ( 'NONE',  ( 3.756430356249995661, -29.49062499938548498, 6.831223922626973533 ) ) ;
#25615 = CARTESIAN_POINT ( 'NONE',  ( 3.735045420075836212E-15, 27.16562499938548569, 4.662447845253954171 ) ) ;
#25617 = EDGE_CURVE ( 'NONE', #18972, #16823, #11821, .T. ) ;
#25616 = LINE ( 'NONE', #1824, #1186 ) ;
#25618 = COLOUR_RGB ( '',0.8941176470588234615, 0.8941176470588234615, 0.8941176470588234615 ) ;
#25619 = CARTESIAN_POINT ( 'NONE',  ( -1.999999999999998224, 26.59374999877096712, 12.46410161513774639 ) ) ;
#25620 = DIRECTION ( 'NONE',  ( 1.000000000000000000, 0.000000000000000000, 0.000000000000000000 ) ) ;
#25621 = EDGE_LOOP ( 'NONE', ( #4584, #4536, #17963, #17214 ) ) ;
#25622 = CARTESIAN_POINT ( 'NONE',  ( 3.999999999999995559, -26.93124999877096926, 6.690598923241487306 ) ) ;
#25623 = CYLINDRICAL_SURFACE ( 'NONE', #20878, 4.000000000000000000 ) ;
#25625 = EDGE_LOOP ( 'NONE', ( #6742, #14277, #15080, #8916 ) ) ;
#25624 = CARTESIAN_POINT ( 'NONE',  ( -3.834746474454188013E-15, -26.40624999877096357, 4.999999999999992006 ) ) ;
#25626 = ADVANCED_FACE ( 'NONE', ( #5626 ), #19603, .F. ) ;
#25627 = COLOUR_RGB ( '',0.8941176470588234615, 0.8941176470588234615, 0.8941176470588234615 ) ;
#25628 = EDGE_LOOP ( 'NONE', ( #18559, #18844, #3846, #4550 ) ) ;
#25629 = ORIENTED_EDGE ( 'NONE', *, *, #7759, .F. ) ;
#25630 = ORIENTED_EDGE ( 'NONE', *, *, #2505, .T. ) ;
#25631 = EDGE_CURVE ( 'NONE', #1348, #18727, #19450, .T. ) ;
#25632 = ORIENTED_EDGE ( 'NONE', *, *, #7937, .F. ) ;
#25633 = DIRECTION ( 'NONE',  ( 0.000000000000000000, 0.000000000000000000, 1.000000000000000000 ) ) ;
#25634 = DIRECTION ( 'NONE',  ( 0.000000000000000000, 0.000000000000000000, -1.000000000000000000 ) ) ;
#25635 = DIRECTION ( 'NONE',  ( 0.9048270524660262382, 0.4257792915650585042, 0.000000000000000000 ) ) ;
#25636 = CARTESIAN_POINT ( 'NONE',  ( -1.878215178124996498, 25.74062499938548854, 5.746835883940462963 ) ) ;
#25637 = CARTESIAN_POINT ( 'NONE',  ( 2.672651547586948120E-15, -13.33755215474602984, 2.728124999385481253 ) ) ;
#25638 = CARTESIAN_POINT ( 'NONE',  ( 3.752267015613588906E-15, -4.381197846482986158, 1.406249998770964904 ) ) ;
#25639 = CARTESIAN_POINT ( 'NONE',  ( 3.756430356250003655, 29.30312499938548498, 8.999999999999992895 ) ) ;
#25640 = AXIS2_PLACEMENT_3D ( 'NONE', #22961, #16956, #11310 ) ;
#25641 = LINE ( 'NONE', #17156, #13392 ) ;
#25642 = CARTESIAN_POINT ( 'NONE',  ( 18.12403068441868470, 23.78088493391098979, 6.690598923241487306 ) ) ;
#25643 = CARTESIAN_POINT ( 'NONE',  ( 4.000000000000001776, -11.30940107675849760, 1.312499999999998224 ) ) ;
#25644 = CARTESIAN_POINT ( 'NONE',  ( 1.859271017917182139E-15, 28.93749999999999645, 12.99999999999999289 ) ) ;
#25645 = DIRECTION ( 'NONE',  ( 0.000000000000000000, 0.000000000000000000, 1.000000000000000000 ) ) ;
#25646 = DIRECTION ( 'NONE',  ( -0.9685831611286283005, 0.2486898871648657861, 0.000000000000000000 ) ) ;
#25647 =( BOUNDED_CURVE ( )  B_SPLINE_CURVE ( 2, ( #24676, #8862, #6621, #6498, #24811, #14483, #10799, #10937, #10547 ),
 .UNSPECIFIED., .F., .T. ) 
 B_SPLINE_CURVE_WITH_KNOTS ( ( 3, 2, 2, 2, 3 ),
 ( 0.5750000000000000666, 0.5833333333333333703, 0.5999999999999999778, 0.6166666666666666963, 0.6250000000000000000 ),
 .UNSPECIFIED. ) 
 CURVE ( )  GEOMETRIC_REPRESENTATION_ITEM ( )  RATIONAL_B_SPLINE_CURVE ( ( 0.9330127018922194093, 0.9330127018922198534, 1.000000000000000000, 0.8660254037844387076, 1.000000000000000000, 0.8660254037844387076, 1.000000000000000000, 0.9330127018922194093, 0.9330127018922194093 ) ) 
 REPRESENTATION_ITEM ( '' )  );
#25648 = CARTESIAN_POINT ( 'NONE',  ( -2.000000000000000888, -26.66874999877096641, 12.46410161513774817 ) ) ;
#25649 = CARTESIAN_POINT ( 'NONE',  ( -1.878215178124998497, 28.70312499938548356, 12.25316411605951927 ) ) ;
#25650 = CARTESIAN_POINT ( 'NONE',  ( -19.82388608118395013, 23.96296185032730364, -6.500000000000000000 ) ) ;
#25651 = CARTESIAN_POINT ( 'NONE',  ( -27.64012133169306296, 13.24173596767408867, 1.000000000000000000 ) ) ;
#25652 = CARTESIAN_POINT ( 'NONE',  ( 18.28012134629577190, -25.16042852506097205, -6.500000000000000000 ) ) ;
#25653 = ORIENTED_EDGE ( 'NONE', *, *, #13308, .T. ) ;
#25654 = CARTESIAN_POINT ( 'NONE',  ( -3.999999999999996447, 27.06250000000000000, 11.30940107675849404 ) ) ;
#25655 = ORIENTED_EDGE ( 'NONE', *, *, #12593, .F. ) ;
#25656 =( BOUNDED_CURVE ( )  B_SPLINE_CURVE ( 2, ( #4181, #21850, #14127 ),
 .UNSPECIFIED., .F., .F. ) 
 B_SPLINE_CURVE_WITH_KNOTS ( ( 3, 3 ),
 ( 0.9889400238386636399, 1.000000000000000000 ),
 .UNSPECIFIED. ) 
 CURVE ( )  GEOMETRIC_REPRESENTATION_ITEM ( )  RATIONAL_B_SPLINE_CURVE ( ( 0.9401842259098239785, 0.9110946495778740051, 1.000000000000000000 ) ) 
 REPRESENTATION_ITEM ( '' )  );
#25657 = ORIENTED_EDGE ( 'NONE', *, *, #15600, .F. ) ;
#25658 = CARTESIAN_POINT ( 'NONE',  ( 0.000000000000000000, 0.000000000000000000, -6.500000000000000000 ) ) ;
#25659 = ORIENTED_EDGE ( 'NONE', *, *, #20142, .F. ) ;
#25660 = CARTESIAN_POINT ( 'NONE',  ( 1.878215178124998497, -27.35312499938548569, 12.25316411605951927 ) ) ;
#25661 = EDGE_CURVE ( 'NONE', #3018, #11616, #147, .T. ) ;
#25662 = ORIENTED_EDGE ( 'NONE', *, *, #20514, .T. ) ;
#25663 = CARTESIAN_POINT ( 'NONE',  ( 0.000000000000000000, 0.000000000000000000, -6.500000000000000000 ) ) ;
#25664 = ADVANCED_FACE ( 'NONE', ( #1452 ), #17526, .T. ) ;
#25665 = ORIENTED_EDGE ( 'NONE', *, *, #2801, .T. ) ;
#25666 = CARTESIAN_POINT ( 'NONE',  ( 4.000000000000001776, 27.66249999999999787, 11.30940107675849760 ) ) ;
#25667 = EDGE_CURVE ( 'NONE', #21691, #25423, #21846, .T. ) ;
#25668 = CARTESIAN_POINT ( 'NONE',  ( 26.49999999999999645, -0.5000000000000000000, 19.00000000000000000 ) ) ;
#25669 = CARTESIAN_POINT ( 'NONE',  ( -3.756430356249995661, -6.831223922626973533, 1.340624999385481075 ) ) ;
#25670 = DIRECTION ( 'NONE',  ( 0.000000000000000000, 0.000000000000000000, 1.000000000000000000 ) ) ;
#25671 = CARTESIAN_POINT ( 'NONE',  ( 21.35910797434536335, 18.70291059638591946, 12.25316411605952283 ) ) ;
#25672 = CARTESIAN_POINT ( 'NONE',  ( -30.54913349766215802, 5.827558883616378083, -6.500000000000000000 ) ) ;
#25673 = CARTESIAN_POINT ( 'NONE',  ( 4.000000000000005329, 28.99374999877097281, 8.999999999999992895 ) ) ;
#25674 = CARTESIAN_POINT ( 'NONE',  ( -3.999999999999996447, 27.02500000000000213, 8.999999999999992895 ) ) ;
#25675 = CARTESIAN_POINT ( 'NONE',  ( 2.620986760973688460E-15, -13.61880215351699874, 3.487499999999998934 ) ) ;
#25676 = DIRECTION ( 'NONE',  ( 1.000000000000000000, 0.000000000000000000, 0.000000000000000000 ) ) ;
#25677 = CARTESIAN_POINT ( 'NONE',  ( 17.08421000182759997, -25.98730014090448392, -2.750000000000000000 ) ) ;
#25678 = ORIENTED_EDGE ( 'NONE', *, *, #1575, .F. ) ;
#25679 = ORIENTED_EDGE ( 'NONE', *, *, #15303, .F. ) ;
#25680 = CARTESIAN_POINT ( 'NONE',  ( -1.999999999999994893, 29.59374999877097068, 5.535898384862237620 ) ) ;
#25681 = ORIENTED_EDGE ( 'NONE', *, *, #25697, .F. ) ;
#25682 = CARTESIAN_POINT ( 'NONE',  ( -1.999999999999995781, 25.99374999877096926, 5.535898384862237620 ) ) ;
#25683 = EDGE_CURVE ( 'NONE', #6382, #19275, #3789, .T. ) ;
#25684 = CARTESIAN_POINT ( 'NONE',  ( -1.878215178124995832, 29.45312499938548356, 5.746835883940462963 ) ) ;
#25685 = CARTESIAN_POINT ( 'NONE',  ( 17.01355443044479898, 18.52930395829678289, 4.999999999999992895 ) ) ;
#25686 = ORIENTED_EDGE ( 'NONE', *, *, #13214, .T. ) ;
#25687 = EDGE_LOOP ( 'NONE', ( #13266, #9535, #24518, #18255 ) ) ;
#25688 = EDGE_CURVE ( 'NONE', #20633, #4730, #13354, .T. ) ;
#25689 = DIRECTION ( 'NONE',  ( 0.000000000000000000, 0.000000000000000000, 1.000000000000000000 ) ) ;
#25690 = ORIENTED_EDGE ( 'NONE', *, *, #19030, .T. ) ;
#25691 = PLANE ( 'NONE',  #11398 ) ;
#25692 = DIRECTION ( 'NONE',  ( 0.000000000000000000, 0.000000000000000000, 1.000000000000000000 ) ) ;
#25693 = CARTESIAN_POINT ( 'NONE',  ( -1.878215178124996498, 27.09062499938548996, 5.746835883940462963 ) ) ;
#25694 = B_SPLINE_CURVE_WITH_KNOTS ( 'NONE', 3,
 ( #23398, #3524, #7057, #15044, #23024, #5109, #17512, #23532, #17896, #5732, #16078, #11614, #21689, #13712 ),
 .UNSPECIFIED., .F., .F.,
 ( 4, 2, 2, 2, 2, 2, 4 ),
 ( 0.0001914289244202972522, 0.0006076524577255098137, 0.0008157642243781109987, 0.001023875991030711967, 0.001231987757683313152, 0.001440099524335914337, 0.001856323057641129934 ),
 .UNSPECIFIED. ) ;
#25695 = CARTESIAN_POINT ( 'NONE',  ( 3.469446951953614189E-15, 40.00000000000000000, 8.999999999999992895 ) ) ;
#25696 = CARTESIAN_POINT ( 'NONE',  ( -1.999999999999994893, 27.40000000000000213, 5.535898384862237620 ) ) ;
#25697 = EDGE_CURVE ( 'NONE', #13143, #15567, #19221, .T. ) ;
#25698 = CARTESIAN_POINT ( 'NONE',  ( -3.756430356249996994, 25.36562499938548498, 8.999999999999992895 ) ) ;
#25699 = CARTESIAN_POINT ( 'NONE',  ( -1.071796769724481901, 27.56740381056766864, 12.99999999999999645 ) ) ;
#25700 = VECTOR ( 'NONE', #4320, 1000.000000000000000 ) ;
#25701 = AXIS2_PLACEMENT_3D ( 'NONE', #18850, #24734, #4736 ) ;
#25702 = CARTESIAN_POINT ( 'NONE',  ( -3.874271733779039106, 38.57135925840245960, 4.512371625048121615 ) ) ;
#25703 = CARTESIAN_POINT ( 'NONE',  ( 17.00591808753650724, 19.83434521228262426, 5.535898384862237620 ) ) ;
#25704 = CARTESIAN_POINT ( 'NONE',  ( 19.84539375530421168, 19.84539375530412997, 4.662447845253954171 ) ) ;
#25705 = CYLINDRICAL_SURFACE ( 'NONE', #21777, 0.5000000000000004441 ) ;
#25706 = CARTESIAN_POINT ( 'NONE',  ( 31.09598070739550479, -0.4999838450260850053, -2.750000000000000000 ) ) ;
#25707 = CARTESIAN_POINT ( 'NONE',  ( 21.58253194665774188, 20.83893265812701046, 5.025965267902964939 ) ) ;
#25708 = CARTESIAN_POINT ( 'NONE',  ( 22.97888821056449515, 17.66649345464567489, 8.999999999999992895 ) ) ;
#25709 = CARTESIAN_POINT ( 'NONE',  ( 3.878215178125003604, 29.57031249969274356, 8.999999999999992895 ) ) ;
#25710 = ORIENTED_EDGE ( 'NONE', *, *, #18126, .T. ) ;
#25711 = CARTESIAN_POINT ( 'NONE',  ( -3.999999999999996447, 27.86874999877096570, 8.999999999999992895 ) ) ;
#25712 = CARTESIAN_POINT ( 'NONE',  ( -4.000000000000003553, -25.48750000000000071, 6.690598923241489970 ) ) ;
#25713 = ORIENTED_EDGE ( 'NONE', *, *, #5842, .F. ) ;
#25714 = CARTESIAN_POINT ( 'NONE',  ( -1.878215178124995832, 28.10312499938548569, 5.746835883940462963 ) ) ;
#25715 = CARTESIAN_POINT ( 'NONE',  ( -9.610428525060479288, 29.57785765677940404, -6.500000000000000000 ) ) ;
#25716 = ADVANCED_FACE ( 'NONE', ( #1320 ), #24356, .T. ) ;
#25717 = ORIENTED_EDGE ( 'NONE', *, *, #13013, .F. ) ;
#25718 = DIRECTION ( 'NONE',  ( 0.000000000000000000, 0.000000000000000000, 1.000000000000000000 ) ) ;
#25719 = ORIENTED_EDGE ( 'NONE', *, *, #3811, .T. ) ;
#25720 = ORIENTED_EDGE ( 'NONE', *, *, #202, .F. ) ;
#25721 = LINE ( 'NONE', #17875, #18094 ) ;
#25722 = CARTESIAN_POINT ( 'NONE',  ( -1.878215178124999829, 26.34062499938548996, 12.25316411605951927 ) ) ;
#25723 = EDGE_CURVE ( 'NONE', #485, #10079, #23936, .T. ) ;
#25724 = CARTESIAN_POINT ( 'NONE',  ( 3.735045420075836212E-15, -4.662447845253954171, 3.853124999385482585 ) ) ;
#25725 = CARTESIAN_POINT ( 'NONE',  ( -1.071796769724483234, 28.41115380933863577, 12.99999999999999645 ) ) ;
#25726 =( NAMED_UNIT ( * ) PLANE_ANGLE_UNIT ( ) SI_UNIT ( $, .RADIAN. ) );
#25727 = DIRECTION ( 'NONE',  ( 0.000000000000000000, 0.000000000000000000, 1.000000000000000000 ) ) ;
#25728 = CARTESIAN_POINT ( 'NONE',  ( 4.000000000000003553, 29.69687499938548569, 8.999999999999992895 ) ) ;
#25729 = DIRECTION ( 'NONE',  ( -1.000000000000000000, 0.000000000000000000, 0.000000000000000000 ) ) ;
#25730 = CARTESIAN_POINT ( 'NONE',  ( 4.000000000000001776, 28.56249999999999645, 11.30940107675849760 ) ) ;
#25731 = CARTESIAN_POINT ( 'NONE',  ( 18.17485398475098535, 18.17485398475091785, 4.662447845253954171 ) ) ;
#25732 = LINE ( 'NONE', #13839, #1353 ) ;
#25733 = EDGE_LOOP ( 'NONE', ( #15723, #8382, #7318, #21373, #7372, #9737, #7816, #222, #19135, #12710, #10205, #4000, #9946, #4974, #11431, #12035, #6996, #1085, #25748, #1472, #19914, #3696, #2493, #12358 ) ) ;
#25734 = CARTESIAN_POINT ( 'NONE',  ( -5.244799308578346420, 38.86679461760645182, 11.05583806265907754 ) ) ;
#25735 = CARTESIAN_POINT ( 'NONE',  ( 5.312745220820863423, 38.96942687711479891, 7.461705451413530810 ) ) ;
#25736 = CARTESIAN_POINT ( 'NONE',  ( 1.878215178125004048, 28.47812499938548569, 5.746835883940462963 ) ) ;
#25737 = CARTESIAN_POINT ( 'NONE',  ( -1.071796769724488563, 29.76115380933863364, 12.99999999999999289 ) ) ;
#25738 = CARTESIAN_POINT ( 'NONE',  ( -1.999999999999996669, 29.29374999877097707, 12.46410161513774639 ) ) ;
#25739 = DIRECTION ( 'NONE',  ( 1.000000000000000000, 0.000000000000000000, 0.000000000000000000 ) ) ;
#25740 = ORIENTED_EDGE ( 'NONE', *, *, #15408, .F. ) ;
#25741 = CARTESIAN_POINT ( 'NONE',  ( 3.999999999999997335, -27.00624999877096855, 11.30940107675849404 ) ) ;
#25742 = FACE_OUTER_BOUND ( 'NONE', #9295, .T. ) ;
#25744 = ORIENTED_EDGE ( 'NONE', *, *, #4489, .T. ) ;
#25743 = CARTESIAN_POINT ( 'NONE',  ( -8.831537335106614961E-15, -26.63124999877096855, 12.99999999999999112 ) ) ;
#25745 = ORIENTED_EDGE ( 'NONE', *, *, #1122, .T. ) ;
#25746 = ORIENTED_EDGE ( 'NONE', *, *, #7935, .T. ) ;
#25747 = ORIENTED_EDGE ( 'NONE', *, *, #12019, .F. ) ;
#25748 = ORIENTED_EDGE ( 'NONE', *, *, #5402, .F. ) ;
#25749 = CARTESIAN_POINT ( 'NONE',  ( 18.67203843983824996, 18.67203843983818246, 4.999999999999991118 ) ) ;
#25750 = DIRECTION ( 'NONE',  ( -0.000000000000000000, -0.000000000000000000, 1.000000000000000000 ) ) ;
#25751 = EDGE_CURVE ( 'NONE', #23155, #7696, #1390, .T. ) ;
#25752 = CARTESIAN_POINT ( 'NONE',  ( 8.831537335106614961E-15, 26.63124999877096855, 12.99999999999999112 ) ) ;
#25753 = CARTESIAN_POINT ( 'NONE',  ( 6.009258394948636914E-15, 27.50312499938549138, 4.662447845253954171 ) ) ;
#25754 = EDGE_CURVE ( 'NONE', #25535, #22864, #22562, .T. ) ;
#25755 = CARTESIAN_POINT ( 'NONE',  ( -3.756430356249996994, -8.999999999999992895, 2.615624999385480987 ) ) ;
#25756 = CARTESIAN_POINT ( 'NONE',  ( -1.999999999999995781, -5.535898384862237620, 3.243749998770965703 ) ) ;
#25757 = LINE ( 'NONE', #19225, #24796 ) ;
#25758 = ADVANCED_FACE ( 'NONE', ( #18627 ), #12348, .F. ) ;
#25759 = CARTESIAN_POINT ( 'NONE',  ( 3.756430356250002323, 27.91562499938548569, 11.16877607737301226 ) ) ;
#25760 = DIRECTION ( 'NONE',  ( 0.000000000000000000, 1.000000000000000000, 0.000000000000000000 ) ) ;
#25761 = DIRECTION ( 'NONE',  ( 1.000000000000000000, 0.000000000000000000, 0.000000000000000000 ) ) ;
#25762 = CARTESIAN_POINT ( 'NONE',  ( 2.000000000000003997, -5.535898384862238508, 2.774999999999999467 ) ) ;
#25763 = LINE ( 'NONE', #9814, #12103 ) ;
#25765 = ADVANCED_FACE ( 'NONE', ( #24505 ), #18017, .F. ) ;
#25764 = CARTESIAN_POINT ( 'NONE',  ( 2.000000000000003553, 26.36874999877097281, 5.535898384862238508 ) ) ;
#25766 = CYLINDRICAL_SURFACE ( 'NONE', #21805, 0.5000000000000004441 ) ;
#25767 = CARTESIAN_POINT ( 'NONE',  ( 3.999999999999996003, -26.03124999877097068, 6.690598923241487306 ) ) ;
#25768 = CARTESIAN_POINT ( 'NONE',  ( -1.878215178124998497, 26.90312499938548285, 12.25316411605951927 ) ) ;
#25769 = DIRECTION ( 'NONE',  ( -0.3090169943749382919, 0.9510565162951566398, 0.000000000000000000 ) ) ;
#25770 = CYLINDRICAL_SURFACE ( 'NONE', #25019, 4.000000000000000000 ) ;
#25771 = FACE_OUTER_BOUND ( 'NONE', #700, .T. ) ;
#25772 = VERTEX_POINT ( 'NONE', #24988 ) ;
#25773 = CARTESIAN_POINT ( 'NONE',  ( 1.071796769724494336, 25.48615380933863150, 4.999999999999992895 ) ) ;
#25774 = ORIENTED_EDGE ( 'NONE', *, *, #22938, .T. ) ;
#25775 = VERTEX_POINT ( 'NONE', #11002 ) ;
#25776 = DIRECTION ( 'NONE',  ( -0.8660254037844397068, 0.4999999999999983347, -0.000000000000000000 ) ) ;
#25777 = ORIENTED_EDGE ( 'NONE', *, *, #14835, .T. ) ;
#25778 = CARTESIAN_POINT ( 'NONE',  ( 1.878215178124998497, -28.25312499938548427, 12.25316411605951927 ) ) ;
#25779 = ORIENTED_EDGE ( 'NONE', *, *, #9801, .F. ) ;
#25780 = CARTESIAN_POINT ( 'NONE',  ( 4.000000000000003553, -8.999999999999992895, 2.643749998770966059 ) ) ;
#25781 = ORIENTED_EDGE ( 'NONE', *, *, #16961, .T. ) ;
#25782 = CARTESIAN_POINT ( 'NONE',  ( -3.999999999999996447, 29.27500000000000213, 8.999999999999992895 ) ) ;
#25783 = DIRECTION ( 'NONE',  ( 1.000000000000000000, 0.000000000000000000, 0.000000000000000000 ) ) ;
#25784 = CARTESIAN_POINT ( 'NONE',  ( 2.672651547586948120E-15, -13.33755215474602984, 0.5906249993854855163 ) ) ;
#25785 = CARTESIAN_POINT ( 'NONE',  ( 30.10000000000000142, 0.000000000000000000, -6.500000000000000000 ) ) ;
#25786 = CARTESIAN_POINT ( 'NONE',  ( 21.67730602587931088, 19.02110864791986344, 12.25316411605952283 ) ) ;
#25787 = ADVANCED_FACE ( 'NONE', ( #24597 ), #16771, .F. ) ;
#25788 =( BOUNDED_CURVE ( )  B_SPLINE_CURVE ( 2, ( #14848, #3073, #15111, #21236, #13014, #16941, #23085, #13148, #6986 ),
 .UNSPECIFIED., .F., .F. ) 
 B_SPLINE_CURVE_WITH_KNOTS ( ( 3, 2, 2, 2, 3 ),
 ( 0.4250000000000000444, 0.4333333333333333481, 0.4500000000000000111, 0.4666666666666666741, 0.4750000000000000333 ),
 .UNSPECIFIED. ) 
 CURVE ( )  GEOMETRIC_REPRESENTATION_ITEM ( )  RATIONAL_B_SPLINE_CURVE ( ( 0.9330127018922194093, 0.9330127018922196314, 1.000000000000000000, 0.8660254037844387076, 1.000000000000000000, 0.8660254037844387076, 1.000000000000000000, 0.9330127018922191873, 0.9330127018922194093 ) ) 
 REPRESENTATION_ITEM ( '' )  );
#25789 = DIRECTION ( 'NONE',  ( 1.000000000000000000, 0.000000000000000000, 0.000000000000000000 ) ) ;
#25790 = LINE ( 'NONE', #4913, #22139 ) ;
#25791 = AXIS2_PLACEMENT_3D ( 'NONE', #24776, #14226, #5984 ) ;
#25792 = APPLICATION_PROTOCOL_DEFINITION ( 'draft international standard', 'automotive_design', 1998, #599 ) ;
#25793 = EDGE_CURVE ( 'NONE', #16647, #15841, #804, .T. ) ;
#25794 = CARTESIAN_POINT ( 'NONE',  ( -3.999999999999997335, 27.06250000000000000, 11.30940107675849404 ) ) ;
#25795 =( BOUNDED_CURVE ( )  B_SPLINE_CURVE ( 2, ( #18477, #12576, #20286, #14299, #2767, #174, #18599, #2382, #6168 ),
 .UNSPECIFIED., .F., .F. ) 
 B_SPLINE_CURVE_WITH_KNOTS ( ( 3, 2, 2, 2, 3 ),
 ( 0.8249999999999999556, 0.8333333333333333703, 0.8499999999999999778, 0.8666666666666666963, 0.8750000000000000000 ),
 .UNSPECIFIED. ) 
 CURVE ( )  GEOMETRIC_REPRESENTATION_ITEM ( )  RATIONAL_B_SPLINE_CURVE ( ( 0.9330127018922194093, 0.9330127018922189652, 1.000000000000000000, 0.8660254037844387076, 1.000000000000000000, 0.8660254037844387076, 1.000000000000000000, 0.9330127018922194093, 0.9330127018922194093 ) ) 
 REPRESENTATION_ITEM ( '' )  );
#25796 = EDGE_CURVE ( 'NONE', #311, #25812, #18535, .T. ) ;
#25797 = CARTESIAN_POINT ( 'NONE',  ( -3.999999999999997335, 29.31250000000000000, 11.30940107675849404 ) ) ;
#25798 = CARTESIAN_POINT ( 'NONE',  ( 17.93165849759071762, 23.24405325350938867, 11.16877607737301048 ) ) ;
#25799 = LINE ( 'NONE', #7880, #6582 ) ;
#25800 = ORIENTED_EDGE ( 'NONE', *, *, #5762, .T. ) ;
#25801 = EDGE_LOOP ( 'NONE', ( #22769, #15298, #22331, #24128 ) ) ;
#25802 = CARTESIAN_POINT ( 'NONE',  ( 1.878215178124999829, 25.62812499938549138, 12.25316411605952283 ) ) ;
#25803 = ORIENTED_EDGE ( 'NONE', *, *, #5630, .T. ) ;
#25804 = DIRECTION ( 'NONE',  ( -0.000000000000000000, -0.000000000000000000, 1.000000000000000000 ) ) ;
#25805 = CARTESIAN_POINT ( 'NONE',  ( 3.756430356250004099, 25.74062499938548143, 6.831223922626973533 ) ) ;
#25806 = DIRECTION ( 'NONE',  ( 1.000000000000000000, 0.000000000000000000, 0.000000000000000000 ) ) ;
#25807 = CARTESIAN_POINT ( 'NONE',  ( 28.34936733434196299, -12.78762572734067149, -6.500000000000000000 ) ) ;
#25808 = ORIENTED_EDGE ( 'NONE', *, *, #21422, .T. ) ;
#25809 = ORIENTED_EDGE ( 'NONE', *, *, #7384, .T. ) ;
#25810 = AXIS2_PLACEMENT_3D ( 'NONE', #13502, #14008, #25769 ) ;
#25811 = CARTESIAN_POINT ( 'NONE',  ( -11.44867358849371541, -28.91604871112453168, -6.500000000000000000 ) ) ;
#25812 = VERTEX_POINT ( 'NONE', #7073 ) ;
#25813 = FACE_OUTER_BOUND ( 'NONE', #5649, .T. ) ;
#25814 = FACE_OUTER_BOUND ( 'NONE', #17428, .T. ) ;
#25815 = CARTESIAN_POINT ( 'NONE',  ( -3.756430356249996549, 27.57812499938548356, 6.831223922626973533 ) ) ;
#25816 = AXIS2_PLACEMENT_3D ( 'NONE', #3662, #11779, #2099 ) ;
#25817 = FACE_OUTER_BOUND ( 'NONE', #2984, .T. ) ;
#25818 = CARTESIAN_POINT ( 'NONE',  ( 0.000000000000000000, 0.000000000000000000, -6.500000000000000000 ) ) ;
#25819 = CARTESIAN_POINT ( 'NONE',  ( 4.000000000000002665, 26.76249999999999929, 11.30940107675849760 ) ) ;
#25820 = EDGE_CURVE ( 'NONE', #15394, #1602, #9150, .T. ) ;
#25821 = CARTESIAN_POINT ( 'NONE',  ( -1.878215178124995832, 26.19062499938548427, 5.746835883940462963 ) ) ;
#25822 = SURFACE_STYLE_USAGE ( .BOTH. , #7780 ) ;
#25823 = EDGE_CURVE ( 'NONE', #19628, #12515, #18692, .T. ) ;
#25824 = FACE_OUTER_BOUND ( 'NONE', #25801, .T. ) ;
#25825 = AXIS2_PLACEMENT_3D ( 'NONE', #23912, #5994, #21946 ) ;
#25826 = CARTESIAN_POINT ( 'NONE',  ( -3.819794567562884158, 38.64130726140524530, 4.557674856424296372 ) ) ;
#25827 = CARTESIAN_POINT ( 'NONE',  ( 15.96293558528635081, 21.61978983477866478, 8.999999999999992895 ) ) ;
#25828 = CARTESIAN_POINT ( 'NONE',  ( 22.76675617620853131, 17.45436142028971460, 6.831223922626973533 ) ) ;
#25829 = CARTESIAN_POINT ( 'NONE',  ( -2.000000000000003997, -28.61874999877096926, 5.535898384862238508 ) ) ;
#25830 = CARTESIAN_POINT ( 'NONE',  ( 4.000000000000003553, 29.44374999877096855, 8.999999999999992895 ) ) ;
#25832 = DIRECTION ( 'NONE',  ( 0.000000000000000000, -1.000000000000000000, 0.000000000000000000 ) ) ;
#25831 = VECTOR ( 'NONE', #5262, 1000.000000000000000 ) ;
#25833 = CARTESIAN_POINT ( 'NONE',  ( -5.532151103383257329, 38.49999999999999289, 6.677220593914388935 ) ) ;
#25834 = FACE_OUTER_BOUND ( 'NONE', #7740, .T. ) ;
#25835 = AXIS2_PLACEMENT_3D ( 'NONE', #21816, #7694, #6109 ) ;
#25836 = ORIENTED_EDGE ( 'NONE', *, *, #3390, .T. ) ;
#25837 = CARTESIAN_POINT ( 'NONE',  ( 2.000000000000003997, 28.61874999877096926, 5.535898384862238508 ) ) ;
#25838 = CARTESIAN_POINT ( 'NONE',  ( -2.000000000000003997, -27.32500000000000284, 5.535898384862238508 ) ) ;
#25840 = ORIENTED_EDGE ( 'NONE', *, *, #12249, .T. ) ;
#25839 = CARTESIAN_POINT ( 'NONE',  ( 1.878215178125001605, 26.07812499938549067, 12.25316411605952283 ) ) ;
#25841 = CARTESIAN_POINT ( 'NONE',  ( -3.756430356249996994, 27.27812499938548640, 8.999999999999992895 ) ) ;
#25842 = DIRECTION ( 'NONE',  ( 0.000000000000000000, 0.000000000000000000, 1.000000000000000000 ) ) ;
#25843 = CARTESIAN_POINT ( 'NONE',  ( -11.52193136556785369, 23.36965697125208052, 20.00001200000000168 ) ) ;
#25844 = CARTESIAN_POINT ( 'NONE',  ( 4.143002691484658293E-15, 46.00000000000000000, 14.49999999999999289 ) ) ;
#25845 = ORIENTED_EDGE ( 'NONE', *, *, #17842, .F. ) ;
#25846 = ORIENTED_EDGE ( 'NONE', *, *, #10581, .T. ) ;
#25847 = CARTESIAN_POINT ( 'NONE',  ( 3.756430356250002323, 26.52812499938548640, 6.831223922626973533 ) ) ;
#25848 = VECTOR ( 'NONE', #15741, 1000.000000000000000 ) ;
#25849 = CARTESIAN_POINT ( 'NONE',  ( 3.735045420075836212E-15, -4.662447845253954171, 2.503124999385483385 ) ) ;
#25850 = CIRCLE ( 'NONE', #21258, 31.10000000000000142 ) ;
#25851 = CIRCLE ( 'NONE', #807, 0.4999999999999997780 ) ;
#25852 = CARTESIAN_POINT ( 'NONE',  ( 14.98253926456337837, 27.25313774936414291, -6.500000000000000000 ) ) ;
#25853 = EDGE_CURVE ( 'NONE', #23233, #3781, #7334, .T. ) ;
#25854 = DIRECTION ( 'NONE',  ( -0.000000000000000000, -1.000000000000000000, -0.000000000000000000 ) ) ;
#25855 = DIRECTION ( 'NONE',  ( 0.000000000000000000, 0.000000000000000000, 1.000000000000000000 ) ) ;
#25856 = FACE_OUTER_BOUND ( 'NONE', #17839, .T. ) ;
#25857 = CARTESIAN_POINT ( 'NONE',  ( -25.16042852506064165, 18.28012134629622309, -6.500000000000000000 ) ) ;
#25858 = CARTESIAN_POINT ( 'NONE',  ( 3.469446951953614189E-15, -8.999999999999992895, 18.00000000000000000 ) ) ;
#25859 = CARTESIAN_POINT ( 'NONE',  ( 20.43330379829292198, 15.12090904237410527, 8.999999999999992895 ) ) ;
#25860 = CARTESIAN_POINT ( 'NONE',  ( 15.31328122920215229, 20.97013547869446626, 11.30940107675849404 ) ) ;
#25861 = ORIENTED_EDGE ( 'NONE', *, *, #7069, .T. ) ;
#25862 = CARTESIAN_POINT ( 'NONE',  ( -3.526711513758413297, 38.89679573513893729, 4.645898033752330569 ) ) ;
#25863 = CARTESIAN_POINT ( 'NONE',  ( 1.042539689874651954, 29.98299368898127071, 5.129272290912049392 ) ) ;
#25864 = CARTESIAN_POINT ( 'NONE',  ( 3.735045420075836212E-15, 26.71562499938548640, 4.662447845253954171 ) ) ;
#25865 =( GEOMETRIC_REPRESENTATION_CONTEXT ( 3 ) GLOBAL_UNCERTAINTY_ASSIGNED_CONTEXT ( ( #9131 ) ) GLOBAL_UNIT_ASSIGNED_CONTEXT ( ( #77, #19805, #23607 ) ) REPRESENTATION_CONTEXT ( 'NONE', 'WORKASPACE' ) );
#25866 = EDGE_CURVE ( 'NONE', #14853, #1951, #25757, .T. ) ;
#25867 = CARTESIAN_POINT ( 'NONE',  ( -3.999999999999996447, 29.66874999877096997, 8.999999999999992895 ) ) ;
#25868 = AXIS2_PLACEMENT_3D ( 'NONE', #11108, #1442, #2875 ) ;
#25869 = CARTESIAN_POINT ( 'NONE',  ( -1.071796769724491671, 29.12634618820329990, 4.999999999999995559 ) ) ;
#25870 = LINE ( 'NONE', #23914, #24653 ) ;
#25871 = ORIENTED_EDGE ( 'NONE', *, *, #14564, .F. ) ;
#25872 = CARTESIAN_POINT ( 'NONE',  ( 4.000000000000007105, 26.78124999877097068, 6.690598923241489970 ) ) ;
#25873 = CARTESIAN_POINT ( 'NONE',  ( -1.999999999999995781, 25.99374999877096926, 5.535898384862237620 ) ) ;
#25874 = CARTESIAN_POINT ( 'NONE',  ( -27.64012133169306296, 13.24173596767408867, -6.500000000000000000 ) ) ;
#25875 = DIRECTION ( 'NONE',  ( 1.000000000000000000, 0.000000000000000000, 0.000000000000000000 ) ) ;
#25876 = CARTESIAN_POINT ( 'NONE',  ( 1.878215178124998275, 26.86562499938548854, 12.25316411605952283 ) ) ;
#25877 = NEXT_ASSEMBLY_USAGE_OCCURRENCE ( 'NAUO1', ' ', ' ', #13015, #17976, $ ) ;
#25878 = NEXT_ASSEMBLY_USAGE_OCCURRENCE ( 'NAUO2', ' ', ' ', #13015, #9821, $ ) ;
#25879 = NEXT_ASSEMBLY_USAGE_OCCURRENCE ( 'NAUO3', ' ', ' ', #13015, #1360, $ ) ;
#25880 = NEXT_ASSEMBLY_USAGE_OCCURRENCE ( 'NAUO4', ' ', ' ', #13015, #20341, $ ) ;
#25881 = NEXT_ASSEMBLY_USAGE_OCCURRENCE ( 'NAUO5', ' ', ' ', #13015, #22284, $ ) ;
#25882 = NEXT_ASSEMBLY_USAGE_OCCURRENCE ( 'NAUO6', ' ', ' ', #13015, #24993, $ ) ;
#25883 = NEXT_ASSEMBLY_USAGE_OCCURRENCE ( 'NAUO7', ' ', ' ', #13015, #10273, $ ) ;
#25884 = NEXT_ASSEMBLY_USAGE_OCCURRENCE ( 'NAUO8', ' ', ' ', #13015, #17659, $ ) ;
#25885 = NEXT_ASSEMBLY_USAGE_OCCURRENCE ( 'NAUO9', ' ', ' ', #13015, #229, $ ) ;
#25886 = NEXT_ASSEMBLY_USAGE_OCCURRENCE ( 'NAUO10', ' ', ' ', #13015, #3722, $ ) ;
#25887=COLOUR_RGB('Dark Blue',0.08,0.2,0.34);
#25888=FILL_AREA_STYLE_COLOUR('',#25887);
#25889=FILL_AREA_STYLE('',(#25888));
#25890=SURFACE_STYLE_FILL_AREA(#25889);
#25891=SURFACE_SIDE_STYLE('',(#25890));
#25892=SURFACE_STYLE_USAGE(.BOTH.,#25891);
#25893=PRESENTATION_STYLE_ASSIGNMENT((#25892));
#25894=COLOUR_RGB('Light Blue',0.38,0.62,0.78);
#25895=FILL_AREA_STYLE_COLOUR('',#25894);
#25896=FILL_AREA_STYLE('',(#25895));
#25897=SURFACE_STYLE_FILL_AREA(#25896);
#25898=SURFACE_SIDE_STYLE('',(#25897));
#25899=SURFACE_STYLE_USAGE(.BOTH.,#25898);
#25900=PRESENTATION_STYLE_ASSIGNMENT((#25899));
#25901=COLOUR_RGB('Sky Blue',0.24,0.69,0.87);
#25902=FILL_AREA_STYLE_COLOUR('',#25901);
#25903=FILL_AREA_STYLE('',(#25902));
#25904=SURFACE_STYLE_FILL_AREA(#25903);
#25905=SURFACE_SIDE_STYLE('',(#25904));
#25906=SURFACE_STYLE_USAGE(.BOTH.,#25905);
#25907=PRESENTATION_STYLE_ASSIGNMENT((#25906));
#25908=COLOUR_RGB('Grey',0.48,0.52,0.57);
#25909=FILL_AREA_STYLE_COLOUR('',#25908);
#25910=FILL_AREA_STYLE('',(#25909));
#25911=SURFACE_STYLE_FILL_AREA(#25910);
#25912=SURFACE_SIDE_STYLE('',(#25911));
#25913=SURFACE_STYLE_USAGE(.BOTH.,#25912);
#25914=PRESENTATION_STYLE_ASSIGNMENT((#25913));
#25915=COLOUR_RGB('Black',0.12,0.14,0.17);
#25916=FILL_AREA_STYLE_COLOUR('',#25915);
#25917=FILL_AREA_STYLE('',(#25916));
#25918=SURFACE_STYLE_FILL_AREA(#25917);
#25919=SURFACE_SIDE_STYLE('',(#25918));
#25920=SURFACE_STYLE_USAGE(.BOTH.,#25919);
#25921=PRESENTATION_STYLE_ASSIGNMENT((#25920));
#25922=COLOUR_RGB('Off White',0.89,0.88,0.83);
#25923=FILL_AREA_STYLE_COLOUR('',#25922);
#25924=FILL_AREA_STYLE('',(#25923));
#25925=SURFACE_STYLE_FILL_AREA(#25924);
#25926=SURFACE_SIDE_STYLE('',(#25925));
#25927=SURFACE_STYLE_USAGE(.BOTH.,#25926);
#25928=PRESENTATION_STYLE_ASSIGNMENT((#25927));
ENDSEC;
END-ISO-10303-21;
